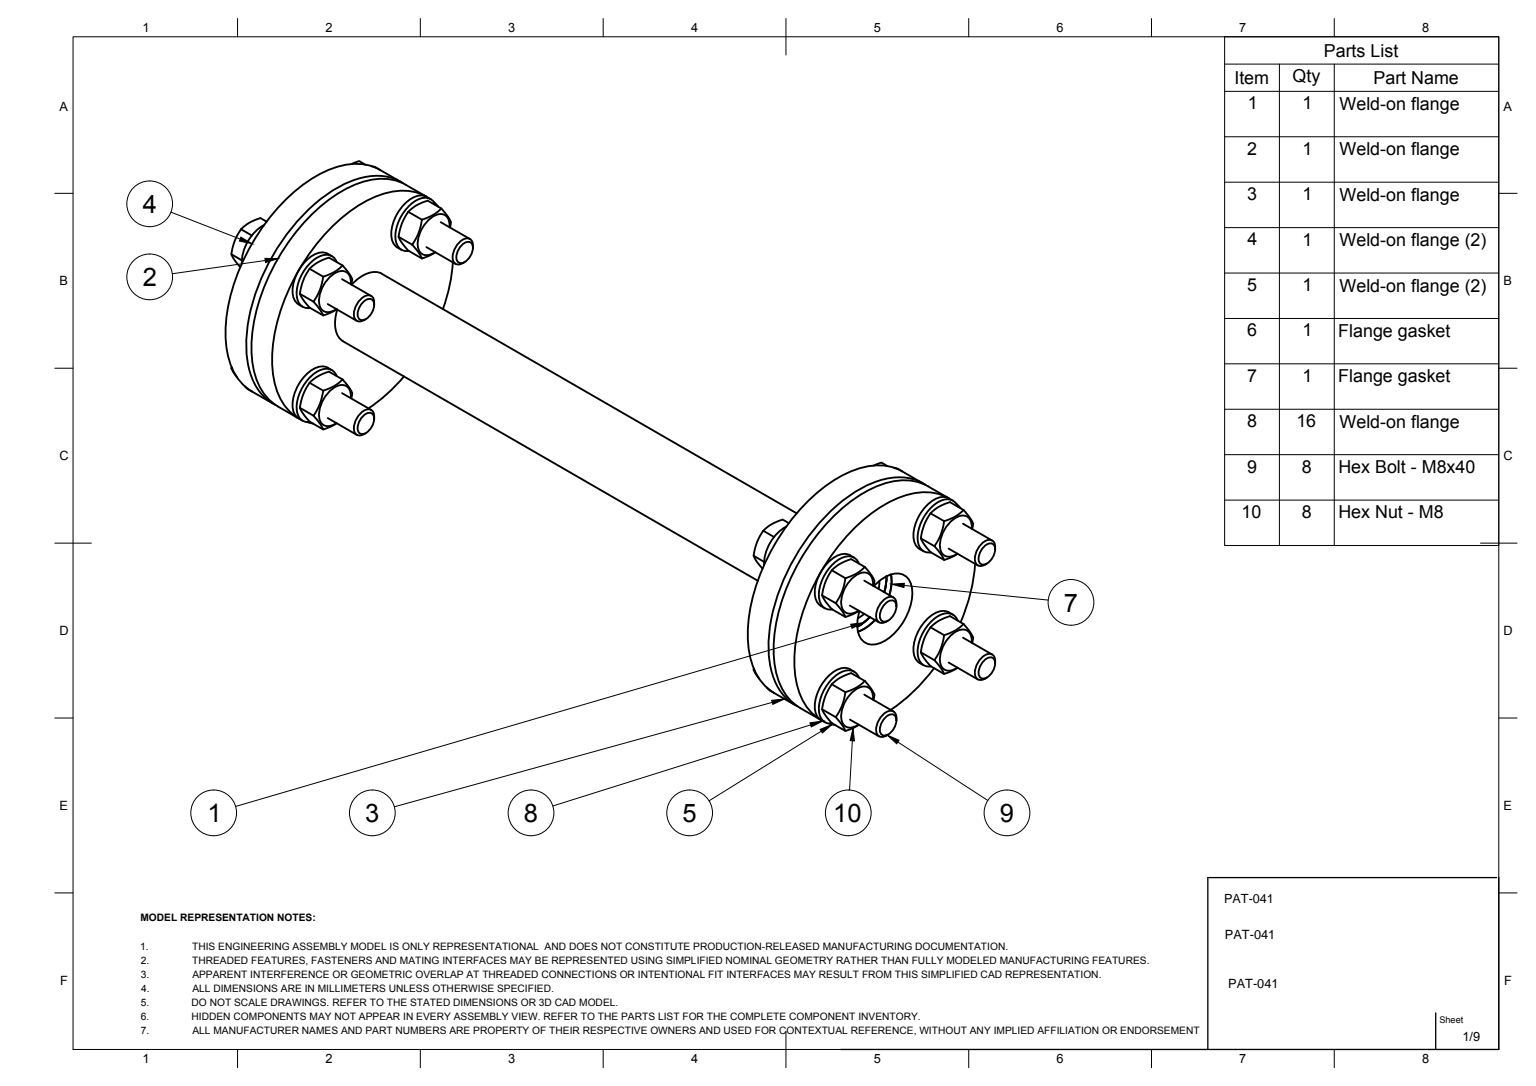
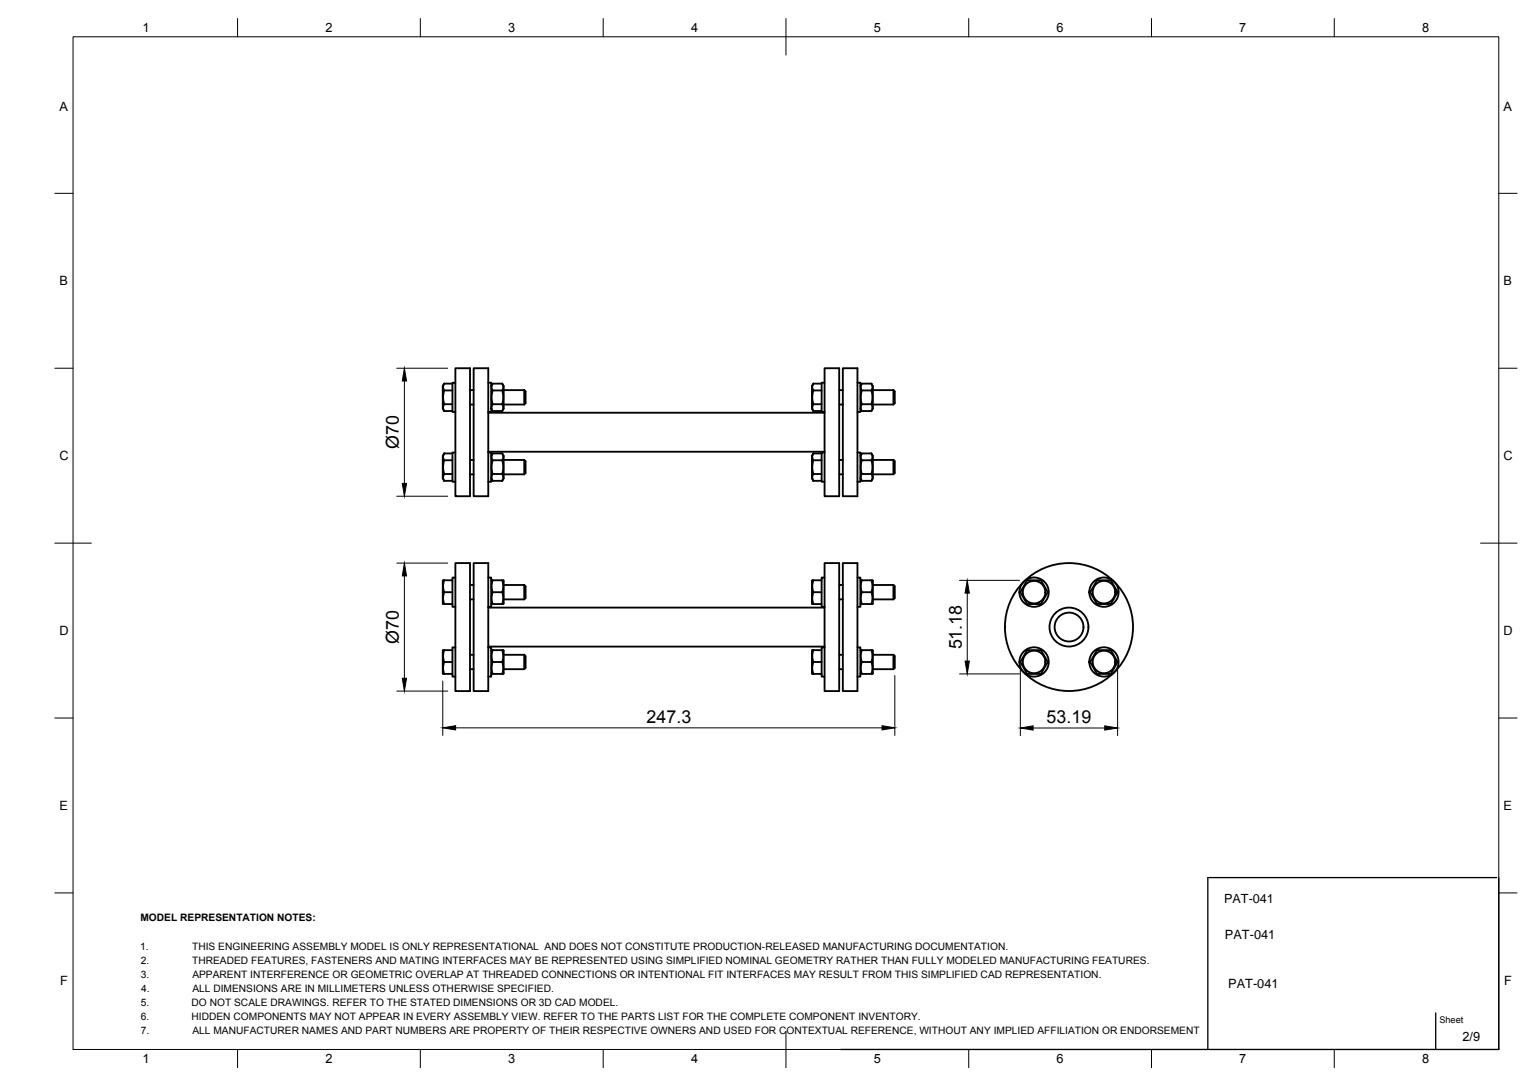
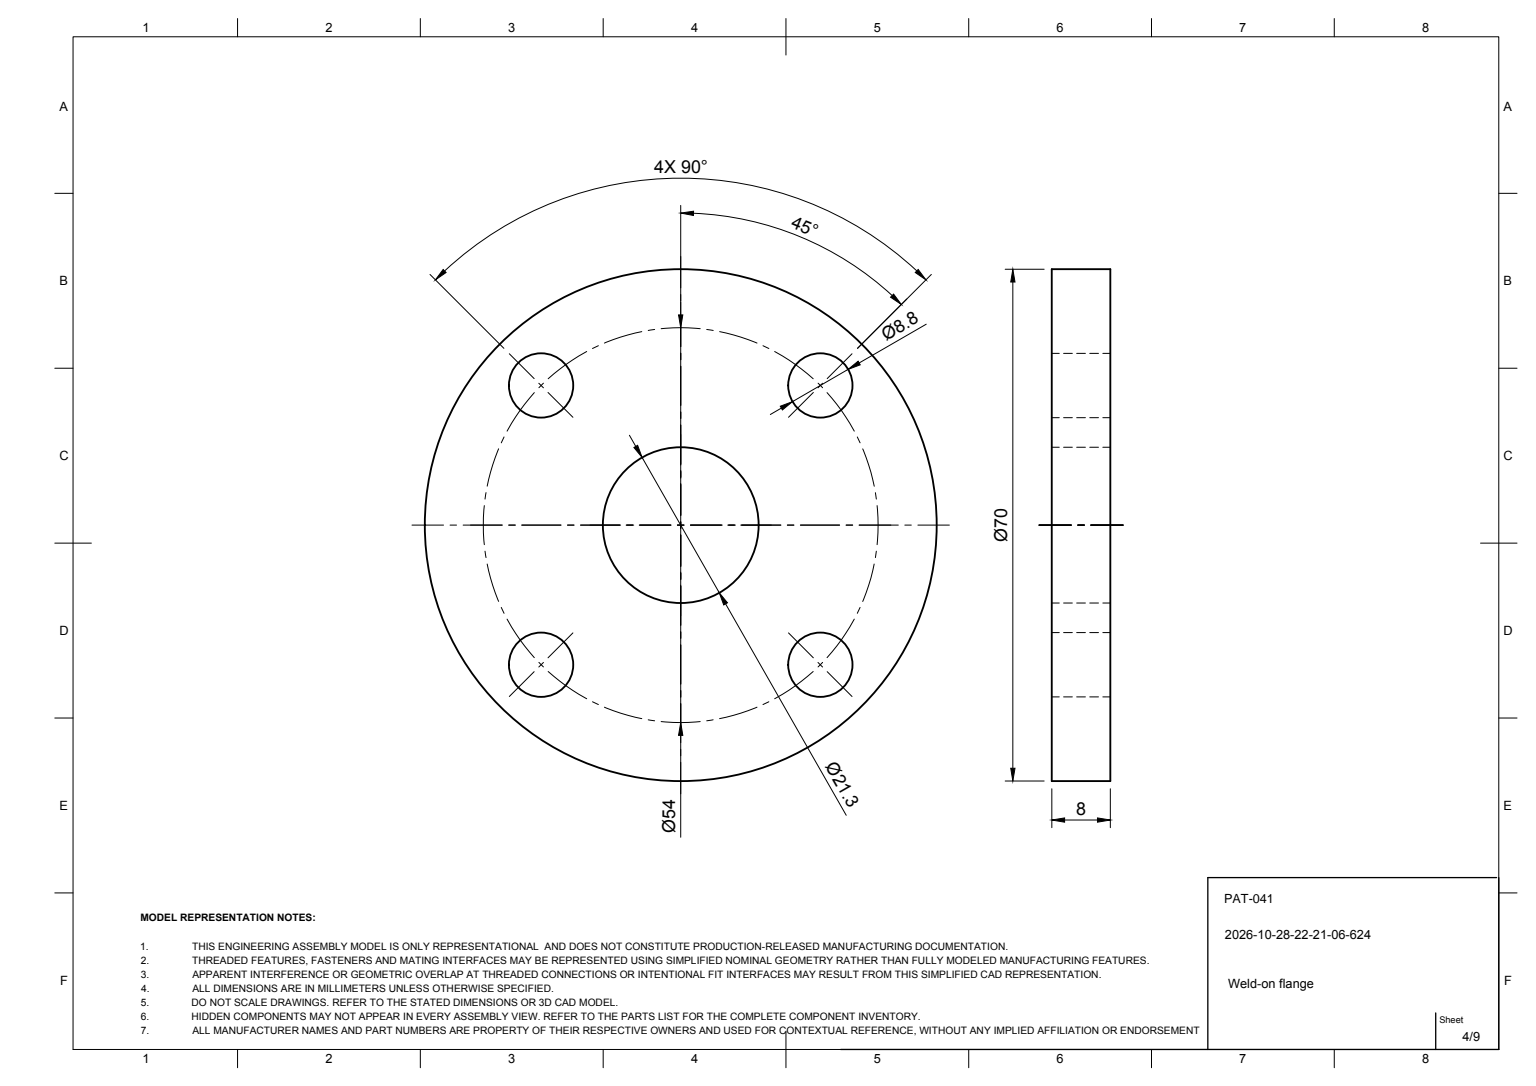
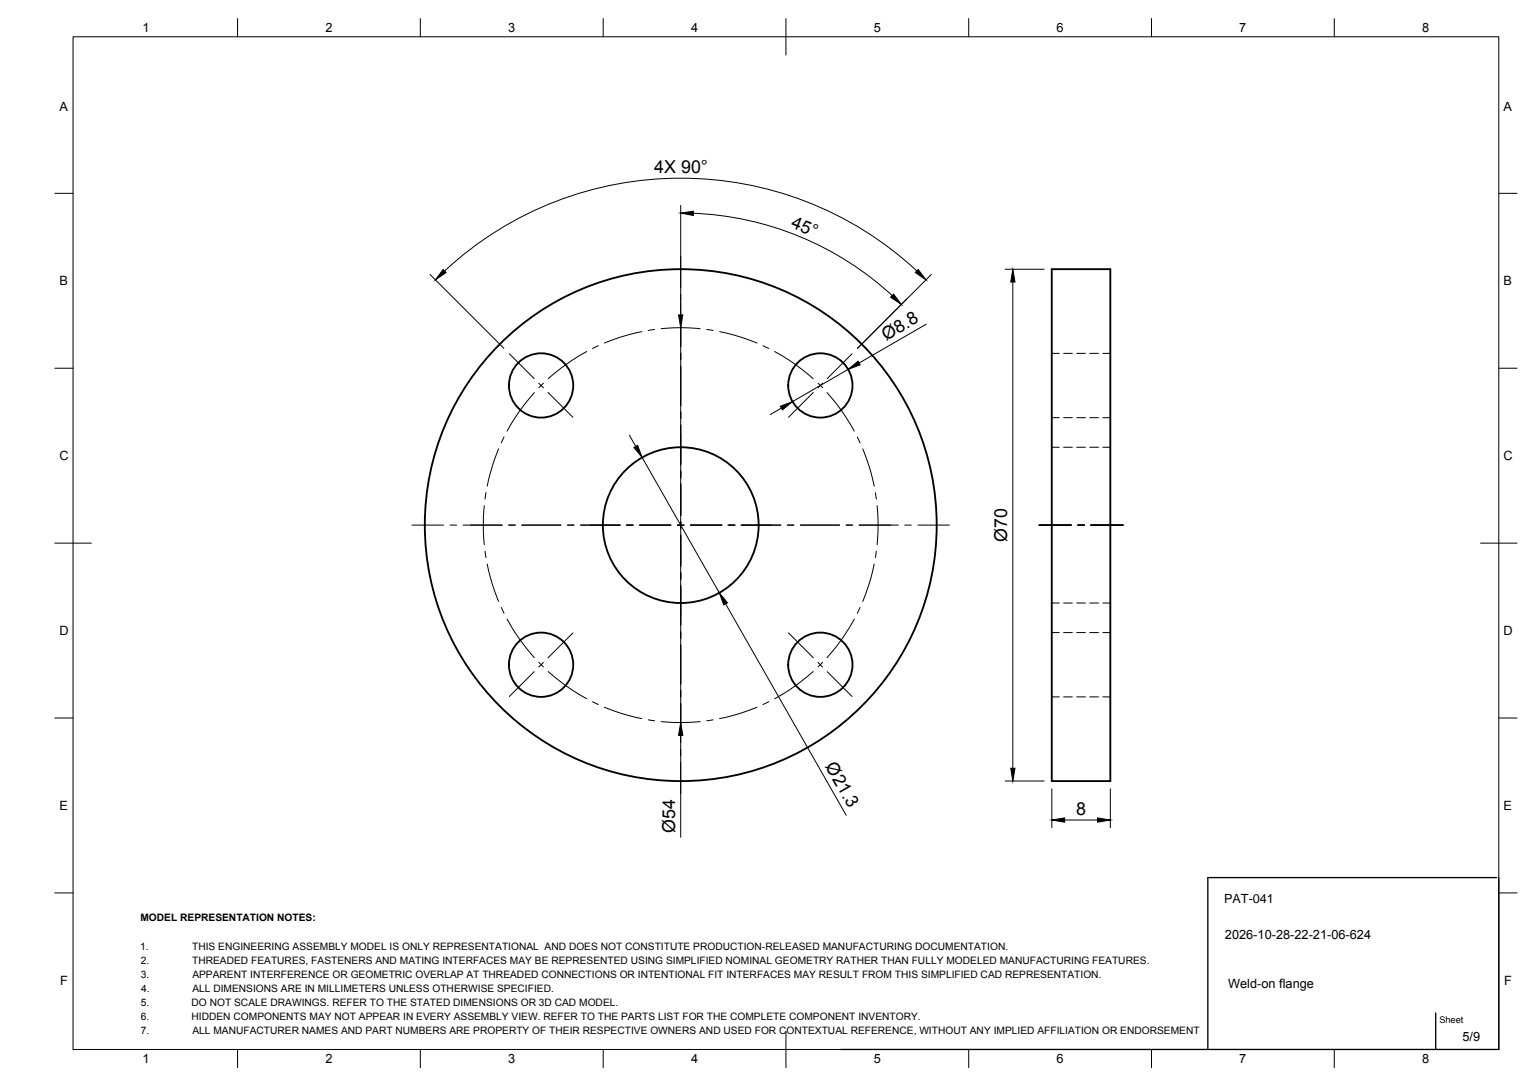
ISO-10303-21;
HEADER;
/* Generated by software containing ST-Developer
 * from STEP Tools, Inc. (www.steptools.com) 
 */

FILE_DESCRIPTION(
/* description */ ('PAT-041'),
/* implementation_level */ '2;1');

FILE_NAME(
/* name */ 'PAT-041',
/* time_stamp */ '2026-10-28T22:21:24-07:00',
/* author */ (''),
/* organization */ (''),
/* preprocessor_version */ 'ST-DEVELOPER v20.2',
/* originating_system */ 'Autodesk Translation Framework v15.17.0.0',
/* authorisation */ '');

FILE_SCHEMA (('AUTOMOTIVE_DESIGN { 1 0 10303 214 3 1 1 }'));
ENDSEC;

DATA;
#10=MECHANICAL_DESIGN_GEOMETRIC_PRESENTATION_REPRESENTATION('',(#209,#210,
#211,#212,#213,#214,#215,#216,#217,#218),#2507);
#11=ITEM_DEFINED_TRANSFORMATION($,$,#1451,#1604);
#12=ITEM_DEFINED_TRANSFORMATION($,$,#1460,#1605);
#13=ITEM_DEFINED_TRANSFORMATION($,$,#1481,#1606);
#14=ITEM_DEFINED_TRANSFORMATION($,$,#1502,#1607);
#15=ITEM_DEFINED_TRANSFORMATION($,$,#1523,#1608);
#16=ITEM_DEFINED_TRANSFORMATION($,$,#1544,#1609);
#17=ITEM_DEFINED_TRANSFORMATION($,$,#1553,#1610);
#18=ITEM_DEFINED_TRANSFORMATION($,$,#1579,#1611);
#19=ITEM_DEFINED_TRANSFORMATION($,$,#1562,#1612);
#20=ITEM_DEFINED_TRANSFORMATION($,$,#1579,#1613);
#21=ITEM_DEFINED_TRANSFORMATION($,$,#1588,#1614);
#22=ITEM_DEFINED_TRANSFORMATION($,$,#1579,#1615);
#23=ITEM_DEFINED_TRANSFORMATION($,$,#1562,#1616);
#24=ITEM_DEFINED_TRANSFORMATION($,$,#1579,#1617);
#25=ITEM_DEFINED_TRANSFORMATION($,$,#1588,#1618);
#26=ITEM_DEFINED_TRANSFORMATION($,$,#1579,#1619);
#27=ITEM_DEFINED_TRANSFORMATION($,$,#1562,#1620);
#28=ITEM_DEFINED_TRANSFORMATION($,$,#1579,#1621);
#29=ITEM_DEFINED_TRANSFORMATION($,$,#1588,#1622);
#30=ITEM_DEFINED_TRANSFORMATION($,$,#1579,#1623);
#31=ITEM_DEFINED_TRANSFORMATION($,$,#1562,#1624);
#32=ITEM_DEFINED_TRANSFORMATION($,$,#1579,#1625);
#33=ITEM_DEFINED_TRANSFORMATION($,$,#1588,#1626);
#34=ITEM_DEFINED_TRANSFORMATION($,$,#1579,#1627);
#35=ITEM_DEFINED_TRANSFORMATION($,$,#1562,#1628);
#36=ITEM_DEFINED_TRANSFORMATION($,$,#1579,#1629);
#37=ITEM_DEFINED_TRANSFORMATION($,$,#1588,#1630);
#38=ITEM_DEFINED_TRANSFORMATION($,$,#1579,#1631);
#39=ITEM_DEFINED_TRANSFORMATION($,$,#1562,#1632);
#40=ITEM_DEFINED_TRANSFORMATION($,$,#1579,#1633);
#41=ITEM_DEFINED_TRANSFORMATION($,$,#1588,#1634);
#42=ITEM_DEFINED_TRANSFORMATION($,$,#1579,#1635);
#43=ITEM_DEFINED_TRANSFORMATION($,$,#1562,#1636);
#44=ITEM_DEFINED_TRANSFORMATION($,$,#1579,#1637);
#45=ITEM_DEFINED_TRANSFORMATION($,$,#1588,#1638);
#46=ITEM_DEFINED_TRANSFORMATION($,$,#1579,#1639);
#47=ITEM_DEFINED_TRANSFORMATION($,$,#1562,#1640);
#48=ITEM_DEFINED_TRANSFORMATION($,$,#1579,#1641);
#49=ITEM_DEFINED_TRANSFORMATION($,$,#1588,#1642);
#50=(
REPRESENTATION_RELATIONSHIP($,$,#2574,#2573)
REPRESENTATION_RELATIONSHIP_WITH_TRANSFORMATION(#11)
SHAPE_REPRESENTATION_RELATIONSHIP()
);
#51=(
REPRESENTATION_RELATIONSHIP($,$,#2575,#2573)
REPRESENTATION_RELATIONSHIP_WITH_TRANSFORMATION(#12)
SHAPE_REPRESENTATION_RELATIONSHIP()
);
#52=(
REPRESENTATION_RELATIONSHIP($,$,#2576,#2573)
REPRESENTATION_RELATIONSHIP_WITH_TRANSFORMATION(#13)
SHAPE_REPRESENTATION_RELATIONSHIP()
);
#53=(
REPRESENTATION_RELATIONSHIP($,$,#2577,#2573)
REPRESENTATION_RELATIONSHIP_WITH_TRANSFORMATION(#14)
SHAPE_REPRESENTATION_RELATIONSHIP()
);
#54=(
REPRESENTATION_RELATIONSHIP($,$,#2578,#2573)
REPRESENTATION_RELATIONSHIP_WITH_TRANSFORMATION(#15)
SHAPE_REPRESENTATION_RELATIONSHIP()
);
#55=(
REPRESENTATION_RELATIONSHIP($,$,#2579,#2573)
REPRESENTATION_RELATIONSHIP_WITH_TRANSFORMATION(#16)
SHAPE_REPRESENTATION_RELATIONSHIP()
);
#56=(
REPRESENTATION_RELATIONSHIP($,$,#2580,#2573)
REPRESENTATION_RELATIONSHIP_WITH_TRANSFORMATION(#17)
SHAPE_REPRESENTATION_RELATIONSHIP()
);
#57=(
REPRESENTATION_RELATIONSHIP($,$,#2582,#2573)
REPRESENTATION_RELATIONSHIP_WITH_TRANSFORMATION(#18)
SHAPE_REPRESENTATION_RELATIONSHIP()
);
#58=(
REPRESENTATION_RELATIONSHIP($,$,#2581,#2573)
REPRESENTATION_RELATIONSHIP_WITH_TRANSFORMATION(#19)
SHAPE_REPRESENTATION_RELATIONSHIP()
);
#59=(
REPRESENTATION_RELATIONSHIP($,$,#2582,#2573)
REPRESENTATION_RELATIONSHIP_WITH_TRANSFORMATION(#20)
SHAPE_REPRESENTATION_RELATIONSHIP()
);
#60=(
REPRESENTATION_RELATIONSHIP($,$,#2583,#2573)
REPRESENTATION_RELATIONSHIP_WITH_TRANSFORMATION(#21)
SHAPE_REPRESENTATION_RELATIONSHIP()
);
#61=(
REPRESENTATION_RELATIONSHIP($,$,#2582,#2573)
REPRESENTATION_RELATIONSHIP_WITH_TRANSFORMATION(#22)
SHAPE_REPRESENTATION_RELATIONSHIP()
);
#62=(
REPRESENTATION_RELATIONSHIP($,$,#2581,#2573)
REPRESENTATION_RELATIONSHIP_WITH_TRANSFORMATION(#23)
SHAPE_REPRESENTATION_RELATIONSHIP()
);
#63=(
REPRESENTATION_RELATIONSHIP($,$,#2582,#2573)
REPRESENTATION_RELATIONSHIP_WITH_TRANSFORMATION(#24)
SHAPE_REPRESENTATION_RELATIONSHIP()
);
#64=(
REPRESENTATION_RELATIONSHIP($,$,#2583,#2573)
REPRESENTATION_RELATIONSHIP_WITH_TRANSFORMATION(#25)
SHAPE_REPRESENTATION_RELATIONSHIP()
);
#65=(
REPRESENTATION_RELATIONSHIP($,$,#2582,#2573)
REPRESENTATION_RELATIONSHIP_WITH_TRANSFORMATION(#26)
SHAPE_REPRESENTATION_RELATIONSHIP()
);
#66=(
REPRESENTATION_RELATIONSHIP($,$,#2581,#2573)
REPRESENTATION_RELATIONSHIP_WITH_TRANSFORMATION(#27)
SHAPE_REPRESENTATION_RELATIONSHIP()
);
#67=(
REPRESENTATION_RELATIONSHIP($,$,#2582,#2573)
REPRESENTATION_RELATIONSHIP_WITH_TRANSFORMATION(#28)
SHAPE_REPRESENTATION_RELATIONSHIP()
);
#68=(
REPRESENTATION_RELATIONSHIP($,$,#2583,#2573)
REPRESENTATION_RELATIONSHIP_WITH_TRANSFORMATION(#29)
SHAPE_REPRESENTATION_RELATIONSHIP()
);
#69=(
REPRESENTATION_RELATIONSHIP($,$,#2582,#2573)
REPRESENTATION_RELATIONSHIP_WITH_TRANSFORMATION(#30)
SHAPE_REPRESENTATION_RELATIONSHIP()
);
#70=(
REPRESENTATION_RELATIONSHIP($,$,#2581,#2573)
REPRESENTATION_RELATIONSHIP_WITH_TRANSFORMATION(#31)
SHAPE_REPRESENTATION_RELATIONSHIP()
);
#71=(
REPRESENTATION_RELATIONSHIP($,$,#2582,#2573)
REPRESENTATION_RELATIONSHIP_WITH_TRANSFORMATION(#32)
SHAPE_REPRESENTATION_RELATIONSHIP()
);
#72=(
REPRESENTATION_RELATIONSHIP($,$,#2583,#2573)
REPRESENTATION_RELATIONSHIP_WITH_TRANSFORMATION(#33)
SHAPE_REPRESENTATION_RELATIONSHIP()
);
#73=(
REPRESENTATION_RELATIONSHIP($,$,#2582,#2573)
REPRESENTATION_RELATIONSHIP_WITH_TRANSFORMATION(#34)
SHAPE_REPRESENTATION_RELATIONSHIP()
);
#74=(
REPRESENTATION_RELATIONSHIP($,$,#2581,#2573)
REPRESENTATION_RELATIONSHIP_WITH_TRANSFORMATION(#35)
SHAPE_REPRESENTATION_RELATIONSHIP()
);
#75=(
REPRESENTATION_RELATIONSHIP($,$,#2582,#2573)
REPRESENTATION_RELATIONSHIP_WITH_TRANSFORMATION(#36)
SHAPE_REPRESENTATION_RELATIONSHIP()
);
#76=(
REPRESENTATION_RELATIONSHIP($,$,#2583,#2573)
REPRESENTATION_RELATIONSHIP_WITH_TRANSFORMATION(#37)
SHAPE_REPRESENTATION_RELATIONSHIP()
);
#77=(
REPRESENTATION_RELATIONSHIP($,$,#2582,#2573)
REPRESENTATION_RELATIONSHIP_WITH_TRANSFORMATION(#38)
SHAPE_REPRESENTATION_RELATIONSHIP()
);
#78=(
REPRESENTATION_RELATIONSHIP($,$,#2581,#2573)
REPRESENTATION_RELATIONSHIP_WITH_TRANSFORMATION(#39)
SHAPE_REPRESENTATION_RELATIONSHIP()
);
#79=(
REPRESENTATION_RELATIONSHIP($,$,#2582,#2573)
REPRESENTATION_RELATIONSHIP_WITH_TRANSFORMATION(#40)
SHAPE_REPRESENTATION_RELATIONSHIP()
);
#80=(
REPRESENTATION_RELATIONSHIP($,$,#2583,#2573)
REPRESENTATION_RELATIONSHIP_WITH_TRANSFORMATION(#41)
SHAPE_REPRESENTATION_RELATIONSHIP()
);
#81=(
REPRESENTATION_RELATIONSHIP($,$,#2582,#2573)
REPRESENTATION_RELATIONSHIP_WITH_TRANSFORMATION(#42)
SHAPE_REPRESENTATION_RELATIONSHIP()
);
#82=(
REPRESENTATION_RELATIONSHIP($,$,#2581,#2573)
REPRESENTATION_RELATIONSHIP_WITH_TRANSFORMATION(#43)
SHAPE_REPRESENTATION_RELATIONSHIP()
);
#83=(
REPRESENTATION_RELATIONSHIP($,$,#2582,#2573)
REPRESENTATION_RELATIONSHIP_WITH_TRANSFORMATION(#44)
SHAPE_REPRESENTATION_RELATIONSHIP()
);
#84=(
REPRESENTATION_RELATIONSHIP($,$,#2583,#2573)
REPRESENTATION_RELATIONSHIP_WITH_TRANSFORMATION(#45)
SHAPE_REPRESENTATION_RELATIONSHIP()
);
#85=(
REPRESENTATION_RELATIONSHIP($,$,#2582,#2573)
REPRESENTATION_RELATIONSHIP_WITH_TRANSFORMATION(#46)
SHAPE_REPRESENTATION_RELATIONSHIP()
);
#86=(
REPRESENTATION_RELATIONSHIP($,$,#2581,#2573)
REPRESENTATION_RELATIONSHIP_WITH_TRANSFORMATION(#47)
SHAPE_REPRESENTATION_RELATIONSHIP()
);
#87=(
REPRESENTATION_RELATIONSHIP($,$,#2582,#2573)
REPRESENTATION_RELATIONSHIP_WITH_TRANSFORMATION(#48)
SHAPE_REPRESENTATION_RELATIONSHIP()
);
#88=(
REPRESENTATION_RELATIONSHIP($,$,#2583,#2573)
REPRESENTATION_RELATIONSHIP_WITH_TRANSFORMATION(#49)
SHAPE_REPRESENTATION_RELATIONSHIP()
);
#89=CONTEXT_DEPENDENT_SHAPE_REPRESENTATION(#50,#2534);
#90=CONTEXT_DEPENDENT_SHAPE_REPRESENTATION(#51,#2535);
#91=CONTEXT_DEPENDENT_SHAPE_REPRESENTATION(#52,#2536);
#92=CONTEXT_DEPENDENT_SHAPE_REPRESENTATION(#53,#2537);
#93=CONTEXT_DEPENDENT_SHAPE_REPRESENTATION(#54,#2538);
#94=CONTEXT_DEPENDENT_SHAPE_REPRESENTATION(#55,#2539);
#95=CONTEXT_DEPENDENT_SHAPE_REPRESENTATION(#56,#2540);
#96=CONTEXT_DEPENDENT_SHAPE_REPRESENTATION(#57,#2541);
#97=CONTEXT_DEPENDENT_SHAPE_REPRESENTATION(#58,#2542);
#98=CONTEXT_DEPENDENT_SHAPE_REPRESENTATION(#59,#2543);
#99=CONTEXT_DEPENDENT_SHAPE_REPRESENTATION(#60,#2544);
#100=CONTEXT_DEPENDENT_SHAPE_REPRESENTATION(#61,#2545);
#101=CONTEXT_DEPENDENT_SHAPE_REPRESENTATION(#62,#2546);
#102=CONTEXT_DEPENDENT_SHAPE_REPRESENTATION(#63,#2547);
#103=CONTEXT_DEPENDENT_SHAPE_REPRESENTATION(#64,#2548);
#104=CONTEXT_DEPENDENT_SHAPE_REPRESENTATION(#65,#2549);
#105=CONTEXT_DEPENDENT_SHAPE_REPRESENTATION(#66,#2550);
#106=CONTEXT_DEPENDENT_SHAPE_REPRESENTATION(#67,#2551);
#107=CONTEXT_DEPENDENT_SHAPE_REPRESENTATION(#68,#2552);
#108=CONTEXT_DEPENDENT_SHAPE_REPRESENTATION(#69,#2553);
#109=CONTEXT_DEPENDENT_SHAPE_REPRESENTATION(#70,#2554);
#110=CONTEXT_DEPENDENT_SHAPE_REPRESENTATION(#71,#2555);
#111=CONTEXT_DEPENDENT_SHAPE_REPRESENTATION(#72,#2556);
#112=CONTEXT_DEPENDENT_SHAPE_REPRESENTATION(#73,#2557);
#113=CONTEXT_DEPENDENT_SHAPE_REPRESENTATION(#74,#2558);
#114=CONTEXT_DEPENDENT_SHAPE_REPRESENTATION(#75,#2559);
#115=CONTEXT_DEPENDENT_SHAPE_REPRESENTATION(#76,#2560);
#116=CONTEXT_DEPENDENT_SHAPE_REPRESENTATION(#77,#2561);
#117=CONTEXT_DEPENDENT_SHAPE_REPRESENTATION(#78,#2562);
#118=CONTEXT_DEPENDENT_SHAPE_REPRESENTATION(#79,#2563);
#119=CONTEXT_DEPENDENT_SHAPE_REPRESENTATION(#80,#2564);
#120=CONTEXT_DEPENDENT_SHAPE_REPRESENTATION(#81,#2565);
#121=CONTEXT_DEPENDENT_SHAPE_REPRESENTATION(#82,#2566);
#122=CONTEXT_DEPENDENT_SHAPE_REPRESENTATION(#83,#2567);
#123=CONTEXT_DEPENDENT_SHAPE_REPRESENTATION(#84,#2568);
#124=CONTEXT_DEPENDENT_SHAPE_REPRESENTATION(#85,#2569);
#125=CONTEXT_DEPENDENT_SHAPE_REPRESENTATION(#86,#2570);
#126=CONTEXT_DEPENDENT_SHAPE_REPRESENTATION(#87,#2571);
#127=CONTEXT_DEPENDENT_SHAPE_REPRESENTATION(#88,#2572);
#128=NEXT_ASSEMBLY_USAGE_OCCURRENCE('Pipe spool:1','Pipe spool:1',
'Pipe spool:1',#2585,#2586,'Pipe spool:1');
#129=NEXT_ASSEMBLY_USAGE_OCCURRENCE('Weld-on flange:1',
'Weld-on flange:1','Weld-on flange:1',#2585,#2587,'Weld-on flange:1');
#130=NEXT_ASSEMBLY_USAGE_OCCURRENCE('Weld-on flange (1):1',
'Weld-on flange (1):1','Weld-on flange (1):1',#2585,#2588,
'Weld-on flange (1):1');
#131=NEXT_ASSEMBLY_USAGE_OCCURRENCE('Weld-on flange (2):1',
'Weld-on flange (2):1','Weld-on flange (2):1',#2585,#2589,
'Weld-on flange (2):1');
#132=NEXT_ASSEMBLY_USAGE_OCCURRENCE('Weld-on flange (3):1',
'Weld-on flange (3):1','Weld-on flange (3):1',#2585,#2590,
'Weld-on flange (3):1');
#133=NEXT_ASSEMBLY_USAGE_OCCURRENCE('Flange gasket:1','Flange gasket:1',
'Flange gasket:1',#2585,#2591,'Flange gasket:1');
#134=NEXT_ASSEMBLY_USAGE_OCCURRENCE('Flange gasket (1):1',
'Flange gasket (1):1','Flange gasket (1):1',#2585,#2592,
'Flange gasket (1):1');
#135=NEXT_ASSEMBLY_USAGE_OCCURRENCE('Flat Washer - M8:1',
'Flat Washer - M8:1','Flat Washer - M8:1',#2585,#2594,
'Flat Washer - M8:1');
#136=NEXT_ASSEMBLY_USAGE_OCCURRENCE('Hex Bolt - M8x40:1',
'Hex Bolt - M8x40:1','Hex Bolt - M8x40:1',#2585,#2593,
'Hex Bolt - M8x40:1');
#137=NEXT_ASSEMBLY_USAGE_OCCURRENCE('Flat Washer - M8:2',
'Flat Washer - M8:2','Flat Washer - M8:2',#2585,#2594,
'Flat Washer - M8:2');
#138=NEXT_ASSEMBLY_USAGE_OCCURRENCE('Hex Nut - M8:1','Hex Nut - M8:1',
'Hex Nut - M8:1',#2585,#2595,'Hex Nut - M8:1');
#139=NEXT_ASSEMBLY_USAGE_OCCURRENCE('Flat Washer - M8:3',
'Flat Washer - M8:3','Flat Washer - M8:3',#2585,#2594,
'Flat Washer - M8:3');
#140=NEXT_ASSEMBLY_USAGE_OCCURRENCE('Hex Bolt - M8x40:2',
'Hex Bolt - M8x40:2','Hex Bolt - M8x40:2',#2585,#2593,
'Hex Bolt - M8x40:2');
#141=NEXT_ASSEMBLY_USAGE_OCCURRENCE('Flat Washer - M8:4',
'Flat Washer - M8:4','Flat Washer - M8:4',#2585,#2594,
'Flat Washer - M8:4');
#142=NEXT_ASSEMBLY_USAGE_OCCURRENCE('Hex Nut - M8:2','Hex Nut - M8:2',
'Hex Nut - M8:2',#2585,#2595,'Hex Nut - M8:2');
#143=NEXT_ASSEMBLY_USAGE_OCCURRENCE('Flat Washer - M8:5',
'Flat Washer - M8:5','Flat Washer - M8:5',#2585,#2594,
'Flat Washer - M8:5');
#144=NEXT_ASSEMBLY_USAGE_OCCURRENCE('Hex Bolt - M8x40:3',
'Hex Bolt - M8x40:3','Hex Bolt - M8x40:3',#2585,#2593,
'Hex Bolt - M8x40:3');
#145=NEXT_ASSEMBLY_USAGE_OCCURRENCE('Flat Washer - M8:6',
'Flat Washer - M8:6','Flat Washer - M8:6',#2585,#2594,
'Flat Washer - M8:6');
#146=NEXT_ASSEMBLY_USAGE_OCCURRENCE('Hex Nut - M8:3','Hex Nut - M8:3',
'Hex Nut - M8:3',#2585,#2595,'Hex Nut - M8:3');
#147=NEXT_ASSEMBLY_USAGE_OCCURRENCE('Flat Washer - M8:7',
'Flat Washer - M8:7','Flat Washer - M8:7',#2585,#2594,
'Flat Washer - M8:7');
#148=NEXT_ASSEMBLY_USAGE_OCCURRENCE('Hex Bolt - M8x40:4',
'Hex Bolt - M8x40:4','Hex Bolt - M8x40:4',#2585,#2593,
'Hex Bolt - M8x40:4');
#149=NEXT_ASSEMBLY_USAGE_OCCURRENCE('Flat Washer - M8:8',
'Flat Washer - M8:8','Flat Washer - M8:8',#2585,#2594,
'Flat Washer - M8:8');
#150=NEXT_ASSEMBLY_USAGE_OCCURRENCE('Hex Nut - M8:4','Hex Nut - M8:4',
'Hex Nut - M8:4',#2585,#2595,'Hex Nut - M8:4');
#151=NEXT_ASSEMBLY_USAGE_OCCURRENCE('Flat Washer - M8:9',
'Flat Washer - M8:9','Flat Washer - M8:9',#2585,#2594,
'Flat Washer - M8:9');
#152=NEXT_ASSEMBLY_USAGE_OCCURRENCE('Hex Bolt - M8x40:5',
'Hex Bolt - M8x40:5','Hex Bolt - M8x40:5',#2585,#2593,
'Hex Bolt - M8x40:5');
#153=NEXT_ASSEMBLY_USAGE_OCCURRENCE('Flat Washer - M8:10',
'Flat Washer - M8:10','Flat Washer - M8:10',#2585,#2594,
'Flat Washer - M8:10');
#154=NEXT_ASSEMBLY_USAGE_OCCURRENCE('Hex Nut - M8:5','Hex Nut - M8:5',
'Hex Nut - M8:5',#2585,#2595,'Hex Nut - M8:5');
#155=NEXT_ASSEMBLY_USAGE_OCCURRENCE('Flat Washer - M8:11',
'Flat Washer - M8:11','Flat Washer - M8:11',#2585,#2594,
'Flat Washer - M8:11');
#156=NEXT_ASSEMBLY_USAGE_OCCURRENCE('Hex Bolt - M8x40:6',
'Hex Bolt - M8x40:6','Hex Bolt - M8x40:6',#2585,#2593,
'Hex Bolt - M8x40:6');
#157=NEXT_ASSEMBLY_USAGE_OCCURRENCE('Flat Washer - M8:12',
'Flat Washer - M8:12','Flat Washer - M8:12',#2585,#2594,
'Flat Washer - M8:12');
#158=NEXT_ASSEMBLY_USAGE_OCCURRENCE('Hex Nut - M8:6','Hex Nut - M8:6',
'Hex Nut - M8:6',#2585,#2595,'Hex Nut - M8:6');
#159=NEXT_ASSEMBLY_USAGE_OCCURRENCE('Flat Washer - M8:13',
'Flat Washer - M8:13','Flat Washer - M8:13',#2585,#2594,
'Flat Washer - M8:13');
#160=NEXT_ASSEMBLY_USAGE_OCCURRENCE('Hex Bolt - M8x40:7',
'Hex Bolt - M8x40:7','Hex Bolt - M8x40:7',#2585,#2593,
'Hex Bolt - M8x40:7');
#161=NEXT_ASSEMBLY_USAGE_OCCURRENCE('Flat Washer - M8:14',
'Flat Washer - M8:14','Flat Washer - M8:14',#2585,#2594,
'Flat Washer - M8:14');
#162=NEXT_ASSEMBLY_USAGE_OCCURRENCE('Hex Nut - M8:7','Hex Nut - M8:7',
'Hex Nut - M8:7',#2585,#2595,'Hex Nut - M8:7');
#163=NEXT_ASSEMBLY_USAGE_OCCURRENCE('Flat Washer - M8:15',
'Flat Washer - M8:15','Flat Washer - M8:15',#2585,#2594,
'Flat Washer - M8:15');
#164=NEXT_ASSEMBLY_USAGE_OCCURRENCE('Hex Bolt - M8x40:8',
'Hex Bolt - M8x40:8','Hex Bolt - M8x40:8',#2585,#2593,
'Hex Bolt - M8x40:8');
#165=NEXT_ASSEMBLY_USAGE_OCCURRENCE('Flat Washer - M8:16',
'Flat Washer - M8:16','Flat Washer - M8:16',#2585,#2594,
'Flat Washer - M8:16');
#166=NEXT_ASSEMBLY_USAGE_OCCURRENCE('Hex Nut - M8:8','Hex Nut - M8:8',
'Hex Nut - M8:8',#2585,#2595,'Hex Nut - M8:8');
#167=(
BOUNDED_CURVE()
B_SPLINE_CURVE(2,(#2305,#2306,#2307),.UNSPECIFIED.,.F.,.F.)
B_SPLINE_CURVE_WITH_KNOTS((3,3),(0.14973948338295,0.97160236658079),
 .UNSPECIFIED.)
CURVE()
GEOMETRIC_REPRESENTATION_ITEM()
RATIONAL_B_SPLINE_CURVE((1.07140024848292,1.23714644374248,1.07140024848292))
REPRESENTATION_ITEM('')
);
#168=(
BOUNDED_CURVE()
B_SPLINE_CURVE(2,(#2309,#2310,#2311),.UNSPECIFIED.,.F.,.F.)
B_SPLINE_CURVE_WITH_KNOTS((3,3),(0.14973948338295,0.97160236658079),
 .UNSPECIFIED.)
CURVE()
GEOMETRIC_REPRESENTATION_ITEM()
RATIONAL_B_SPLINE_CURVE((1.07140024848292,1.23714644374248,1.07140024848292))
REPRESENTATION_ITEM('')
);
#169=(
BOUNDED_CURVE()
B_SPLINE_CURVE(2,(#2313,#2314,#2315),.UNSPECIFIED.,.F.,.F.)
B_SPLINE_CURVE_WITH_KNOTS((3,3),(0.14973948338295,0.97160236658079),
 .UNSPECIFIED.)
CURVE()
GEOMETRIC_REPRESENTATION_ITEM()
RATIONAL_B_SPLINE_CURVE((1.07140024848292,1.23714644374248,1.07140024848292))
REPRESENTATION_ITEM('')
);
#170=(
BOUNDED_CURVE()
B_SPLINE_CURVE(2,(#2317,#2318,#2319),.UNSPECIFIED.,.F.,.F.)
B_SPLINE_CURVE_WITH_KNOTS((3,3),(0.149739483382949,0.971602366580789),
 .UNSPECIFIED.)
CURVE()
GEOMETRIC_REPRESENTATION_ITEM()
RATIONAL_B_SPLINE_CURVE((1.07140024848292,1.23714644374248,1.07140024848292))
REPRESENTATION_ITEM('')
);
#171=(
BOUNDED_CURVE()
B_SPLINE_CURVE(2,(#2321,#2322,#2323),.UNSPECIFIED.,.F.,.F.)
B_SPLINE_CURVE_WITH_KNOTS((3,3),(0.14973948338295,0.971602366580789),
 .UNSPECIFIED.)
CURVE()
GEOMETRIC_REPRESENTATION_ITEM()
RATIONAL_B_SPLINE_CURVE((1.07140024848292,1.23714644374248,1.07140024848292))
REPRESENTATION_ITEM('')
);
#172=(
BOUNDED_CURVE()
B_SPLINE_CURVE(2,(#2324,#2325,#2326),.UNSPECIFIED.,.F.,.F.)
B_SPLINE_CURVE_WITH_KNOTS((3,3),(0.14973948338295,0.97160236658079),
 .UNSPECIFIED.)
CURVE()
GEOMETRIC_REPRESENTATION_ITEM()
RATIONAL_B_SPLINE_CURVE((1.07140024848292,1.23714644374248,1.07140024848292))
REPRESENTATION_ITEM('')
);
#173=(
BOUNDED_CURVE()
B_SPLINE_CURVE(2,(#2372,#2373,#2374),.UNSPECIFIED.,.F.,.F.)
B_SPLINE_CURVE_WITH_KNOTS((3,3),(0.14973948338295,0.97160236658079),
 .UNSPECIFIED.)
CURVE()
GEOMETRIC_REPRESENTATION_ITEM()
RATIONAL_B_SPLINE_CURVE((1.07140024848292,1.23714644374248,1.07140024848292))
REPRESENTATION_ITEM('')
);
#174=(
BOUNDED_CURVE()
B_SPLINE_CURVE(2,(#2376,#2377,#2378),.UNSPECIFIED.,.F.,.F.)
B_SPLINE_CURVE_WITH_KNOTS((3,3),(0.14973948338295,0.971602366580789),
 .UNSPECIFIED.)
CURVE()
GEOMETRIC_REPRESENTATION_ITEM()
RATIONAL_B_SPLINE_CURVE((1.07140024848292,1.23714644374248,1.07140024848292))
REPRESENTATION_ITEM('')
);
#175=(
BOUNDED_CURVE()
B_SPLINE_CURVE(2,(#2383,#2384,#2385),.UNSPECIFIED.,.F.,.F.)
B_SPLINE_CURVE_WITH_KNOTS((3,3),(0.14973948338295,0.97160236658079),
 .UNSPECIFIED.)
CURVE()
GEOMETRIC_REPRESENTATION_ITEM()
RATIONAL_B_SPLINE_CURVE((1.07140024848292,1.23714644374248,1.07140024848292))
REPRESENTATION_ITEM('')
);
#176=(
BOUNDED_CURVE()
B_SPLINE_CURVE(2,(#2387,#2388,#2389),.UNSPECIFIED.,.F.,.F.)
B_SPLINE_CURVE_WITH_KNOTS((3,3),(0.14973948338295,0.97160236658079),
 .UNSPECIFIED.)
CURVE()
GEOMETRIC_REPRESENTATION_ITEM()
RATIONAL_B_SPLINE_CURVE((1.07140024848292,1.23714644374248,1.07140024848292))
REPRESENTATION_ITEM('')
);
#177=(
BOUNDED_CURVE()
B_SPLINE_CURVE(2,(#2391,#2392,#2393),.UNSPECIFIED.,.F.,.F.)
B_SPLINE_CURVE_WITH_KNOTS((3,3),(0.14973948338295,0.971602366580789),
 .UNSPECIFIED.)
CURVE()
GEOMETRIC_REPRESENTATION_ITEM()
RATIONAL_B_SPLINE_CURVE((1.07140024848292,1.23714644374248,1.07140024848292))
REPRESENTATION_ITEM('')
);
#178=(
BOUNDED_CURVE()
B_SPLINE_CURVE(2,(#2394,#2395,#2396),.UNSPECIFIED.,.F.,.F.)
B_SPLINE_CURVE_WITH_KNOTS((3,3),(0.14973948338295,0.97160236658079),
 .UNSPECIFIED.)
CURVE()
GEOMETRIC_REPRESENTATION_ITEM()
RATIONAL_B_SPLINE_CURVE((1.07140024848292,1.23714644374248,1.07140024848292))
REPRESENTATION_ITEM('')
);
#179=(
BOUNDED_CURVE()
B_SPLINE_CURVE(2,(#2403,#2404,#2405),.UNSPECIFIED.,.F.,.F.)
B_SPLINE_CURVE_WITH_KNOTS((3,3),(0.14973948338295,0.97160236658079),
 .UNSPECIFIED.)
CURVE()
GEOMETRIC_REPRESENTATION_ITEM()
RATIONAL_B_SPLINE_CURVE((1.07140024848292,1.23714644374248,1.07140024848292))
REPRESENTATION_ITEM('')
);
#180=(
BOUNDED_CURVE()
B_SPLINE_CURVE(2,(#2407,#2408,#2409),.UNSPECIFIED.,.F.,.F.)
B_SPLINE_CURVE_WITH_KNOTS((3,3),(0.14973948338295,0.97160236658079),
 .UNSPECIFIED.)
CURVE()
GEOMETRIC_REPRESENTATION_ITEM()
RATIONAL_B_SPLINE_CURVE((1.07140024848292,1.23714644374248,1.07140024848292))
REPRESENTATION_ITEM('')
);
#181=(
BOUNDED_CURVE()
B_SPLINE_CURVE(2,(#2411,#2412,#2413),.UNSPECIFIED.,.F.,.F.)
B_SPLINE_CURVE_WITH_KNOTS((3,3),(0.14973948338295,0.971602366580789),
 .UNSPECIFIED.)
CURVE()
GEOMETRIC_REPRESENTATION_ITEM()
RATIONAL_B_SPLINE_CURVE((1.07140024848292,1.23714644374248,1.07140024848292))
REPRESENTATION_ITEM('')
);
#182=(
BOUNDED_CURVE()
B_SPLINE_CURVE(2,(#2415,#2416,#2417),.UNSPECIFIED.,.F.,.F.)
B_SPLINE_CURVE_WITH_KNOTS((3,3),(0.14973948338295,0.97160236658079),
 .UNSPECIFIED.)
CURVE()
GEOMETRIC_REPRESENTATION_ITEM()
RATIONAL_B_SPLINE_CURVE((1.07140024848292,1.23714644374248,1.07140024848292))
REPRESENTATION_ITEM('')
);
#183=(
BOUNDED_CURVE()
B_SPLINE_CURVE(2,(#2419,#2420,#2421),.UNSPECIFIED.,.F.,.F.)
B_SPLINE_CURVE_WITH_KNOTS((3,3),(0.14973948338295,0.97160236658079),
 .UNSPECIFIED.)
CURVE()
GEOMETRIC_REPRESENTATION_ITEM()
RATIONAL_B_SPLINE_CURVE((1.07140024848292,1.23714644374248,1.07140024848292))
REPRESENTATION_ITEM('')
);
#184=(
BOUNDED_CURVE()
B_SPLINE_CURVE(2,(#2422,#2423,#2424),.UNSPECIFIED.,.F.,.F.)
B_SPLINE_CURVE_WITH_KNOTS((3,3),(0.14973948338295,0.971602366580789),
 .UNSPECIFIED.)
CURVE()
GEOMETRIC_REPRESENTATION_ITEM()
RATIONAL_B_SPLINE_CURVE((1.07140024848292,1.23714644374248,1.07140024848292))
REPRESENTATION_ITEM('')
);
#185=CONICAL_SURFACE('',#1566,0.36,0.785398163397451);
#186=CONICAL_SURFACE('',#1569,0.734027674973257,1.0471975511966);
#187=CONICAL_SURFACE('',#1589,0.734027674973257,1.0471975511966);
#188=CONICAL_SURFACE('',#1591,0.734027674973257,1.0471975511966);
#189=SHAPE_REPRESENTATION_RELATIONSHIP('SRR','None',#2574,#199);
#190=SHAPE_REPRESENTATION_RELATIONSHIP('SRR','None',#2575,#200);
#191=SHAPE_REPRESENTATION_RELATIONSHIP('SRR','None',#2576,#201);
#192=SHAPE_REPRESENTATION_RELATIONSHIP('SRR','None',#2577,#202);
#193=SHAPE_REPRESENTATION_RELATIONSHIP('SRR','None',#2578,#203);
#194=SHAPE_REPRESENTATION_RELATIONSHIP('SRR','None',#2579,#204);
#195=SHAPE_REPRESENTATION_RELATIONSHIP('SRR','None',#2580,#205);
#196=SHAPE_REPRESENTATION_RELATIONSHIP('SRR','None',#2581,#206);
#197=SHAPE_REPRESENTATION_RELATIONSHIP('SRR','None',#2582,#207);
#198=SHAPE_REPRESENTATION_RELATIONSHIP('SRR','None',#2583,#208);
#199=ADVANCED_BREP_SHAPE_REPRESENTATION('',(#219),#2497);
#200=ADVANCED_BREP_SHAPE_REPRESENTATION('',(#220),#2498);
#201=ADVANCED_BREP_SHAPE_REPRESENTATION('',(#221),#2499);
#202=ADVANCED_BREP_SHAPE_REPRESENTATION('',(#222),#2500);
#203=ADVANCED_BREP_SHAPE_REPRESENTATION('',(#223),#2501);
#204=ADVANCED_BREP_SHAPE_REPRESENTATION('',(#224),#2502);
#205=ADVANCED_BREP_SHAPE_REPRESENTATION('',(#225),#2503);
#206=ADVANCED_BREP_SHAPE_REPRESENTATION('',(#226),#2504);
#207=ADVANCED_BREP_SHAPE_REPRESENTATION('',(#227),#2505);
#208=ADVANCED_BREP_SHAPE_REPRESENTATION('',(#228),#2506);
#209=STYLED_ITEM('',(#2708),#219);
#210=STYLED_ITEM('',(#2687),#220);
#211=STYLED_ITEM('',(#2687),#221);
#212=STYLED_ITEM('',(#2687),#222);
#213=STYLED_ITEM('',(#2687),#223);
#214=STYLED_ITEM('',(#2708),#224);
#215=STYLED_ITEM('',(#2708),#225);
#216=STYLED_ITEM('',(#2701),#226);
#217=STYLED_ITEM('',(#2701),#227);
#218=STYLED_ITEM('',(#2701),#228);
#219=MANIFOLD_SOLID_BREP('Body1',#1329);
#220=MANIFOLD_SOLID_BREP('Body1',#1330);
#221=MANIFOLD_SOLID_BREP('Body1',#1331);
#222=MANIFOLD_SOLID_BREP('Body1',#1332);
#223=MANIFOLD_SOLID_BREP('Body1',#1333);
#224=MANIFOLD_SOLID_BREP('Body1',#1334);
#225=MANIFOLD_SOLID_BREP('Body1',#1335);
#226=MANIFOLD_SOLID_BREP('Body1',#1336);
#227=MANIFOLD_SOLID_BREP('Body1',#1337);
#228=MANIFOLD_SOLID_BREP('Body1',#1338);
#229=FACE_BOUND('',#387,.T.);
#230=FACE_BOUND('',#389,.T.);
#231=FACE_BOUND('',#397,.T.);
#232=FACE_BOUND('',#398,.T.);
#233=FACE_BOUND('',#399,.T.);
#234=FACE_BOUND('',#400,.T.);
#235=FACE_BOUND('',#401,.T.);
#236=FACE_BOUND('',#403,.T.);
#237=FACE_BOUND('',#404,.T.);
#238=FACE_BOUND('',#405,.T.);
#239=FACE_BOUND('',#406,.T.);
#240=FACE_BOUND('',#407,.T.);
#241=FACE_BOUND('',#415,.T.);
#242=FACE_BOUND('',#416,.T.);
#243=FACE_BOUND('',#417,.T.);
#244=FACE_BOUND('',#418,.T.);
#245=FACE_BOUND('',#419,.T.);
#246=FACE_BOUND('',#421,.T.);
#247=FACE_BOUND('',#422,.T.);
#248=FACE_BOUND('',#423,.T.);
#249=FACE_BOUND('',#424,.T.);
#250=FACE_BOUND('',#425,.T.);
#251=FACE_BOUND('',#433,.T.);
#252=FACE_BOUND('',#434,.T.);
#253=FACE_BOUND('',#435,.T.);
#254=FACE_BOUND('',#436,.T.);
#255=FACE_BOUND('',#437,.T.);
#256=FACE_BOUND('',#439,.T.);
#257=FACE_BOUND('',#440,.T.);
#258=FACE_BOUND('',#441,.T.);
#259=FACE_BOUND('',#442,.T.);
#260=FACE_BOUND('',#443,.T.);
#261=FACE_BOUND('',#451,.T.);
#262=FACE_BOUND('',#452,.T.);
#263=FACE_BOUND('',#453,.T.);
#264=FACE_BOUND('',#454,.T.);
#265=FACE_BOUND('',#455,.T.);
#266=FACE_BOUND('',#457,.T.);
#267=FACE_BOUND('',#458,.T.);
#268=FACE_BOUND('',#459,.T.);
#269=FACE_BOUND('',#460,.T.);
#270=FACE_BOUND('',#461,.T.);
#271=FACE_BOUND('',#465,.T.);
#272=FACE_BOUND('',#467,.T.);
#273=FACE_BOUND('',#471,.T.);
#274=FACE_BOUND('',#473,.T.);
#275=FACE_BOUND('',#486,.T.);
#276=FACE_BOUND('',#490,.T.);
#277=FACE_BOUND('',#492,.T.);
#278=FACE_BOUND('',#503,.T.);
#279=FACE_BOUND('',#505,.T.);
#280=PLANE('',#1458);
#281=PLANE('',#1459);
#282=PLANE('',#1479);
#283=PLANE('',#1480);
#284=PLANE('',#1500);
#285=PLANE('',#1501);
#286=PLANE('',#1521);
#287=PLANE('',#1522);
#288=PLANE('',#1542);
#289=PLANE('',#1543);
#290=PLANE('',#1551);
#291=PLANE('',#1552);
#292=PLANE('',#1560);
#293=PLANE('',#1561);
#294=PLANE('',#1568);
#295=PLANE('',#1571);
#296=PLANE('',#1572);
#297=PLANE('',#1573);
#298=PLANE('',#1574);
#299=PLANE('',#1575);
#300=PLANE('',#1576);
#301=PLANE('',#1577);
#302=PLANE('',#1578);
#303=PLANE('',#1586);
#304=PLANE('',#1587);
#305=PLANE('',#1593);
#306=PLANE('',#1594);
#307=PLANE('',#1595);
#308=PLANE('',#1599);
#309=PLANE('',#1600);
#310=PLANE('',#1601);
#311=PLANE('',#1602);
#312=PLANE('',#1603);
#313=FACE_OUTER_BOUND('',#384,.T.);
#314=FACE_OUTER_BOUND('',#385,.T.);
#315=FACE_OUTER_BOUND('',#386,.T.);
#316=FACE_OUTER_BOUND('',#388,.T.);
#317=FACE_OUTER_BOUND('',#390,.T.);
#318=FACE_OUTER_BOUND('',#391,.T.);
#319=FACE_OUTER_BOUND('',#392,.T.);
#320=FACE_OUTER_BOUND('',#393,.T.);
#321=FACE_OUTER_BOUND('',#394,.T.);
#322=FACE_OUTER_BOUND('',#395,.T.);
#323=FACE_OUTER_BOUND('',#396,.T.);
#324=FACE_OUTER_BOUND('',#402,.T.);
#325=FACE_OUTER_BOUND('',#408,.T.);
#326=FACE_OUTER_BOUND('',#409,.T.);
#327=FACE_OUTER_BOUND('',#410,.T.);
#328=FACE_OUTER_BOUND('',#411,.T.);
#329=FACE_OUTER_BOUND('',#412,.T.);
#330=FACE_OUTER_BOUND('',#413,.T.);
#331=FACE_OUTER_BOUND('',#414,.T.);
#332=FACE_OUTER_BOUND('',#420,.T.);
#333=FACE_OUTER_BOUND('',#426,.T.);
#334=FACE_OUTER_BOUND('',#427,.T.);
#335=FACE_OUTER_BOUND('',#428,.T.);
#336=FACE_OUTER_BOUND('',#429,.T.);
#337=FACE_OUTER_BOUND('',#430,.T.);
#338=FACE_OUTER_BOUND('',#431,.T.);
#339=FACE_OUTER_BOUND('',#432,.T.);
#340=FACE_OUTER_BOUND('',#438,.T.);
#341=FACE_OUTER_BOUND('',#444,.T.);
#342=FACE_OUTER_BOUND('',#445,.T.);
#343=FACE_OUTER_BOUND('',#446,.T.);
#344=FACE_OUTER_BOUND('',#447,.T.);
#345=FACE_OUTER_BOUND('',#448,.T.);
#346=FACE_OUTER_BOUND('',#449,.T.);
#347=FACE_OUTER_BOUND('',#450,.T.);
#348=FACE_OUTER_BOUND('',#456,.T.);
#349=FACE_OUTER_BOUND('',#462,.T.);
#350=FACE_OUTER_BOUND('',#463,.T.);
#351=FACE_OUTER_BOUND('',#464,.T.);
#352=FACE_OUTER_BOUND('',#466,.T.);
#353=FACE_OUTER_BOUND('',#468,.T.);
#354=FACE_OUTER_BOUND('',#469,.T.);
#355=FACE_OUTER_BOUND('',#470,.T.);
#356=FACE_OUTER_BOUND('',#472,.T.);
#357=FACE_OUTER_BOUND('',#474,.T.);
#358=FACE_OUTER_BOUND('',#475,.T.);
#359=FACE_OUTER_BOUND('',#476,.T.);
#360=FACE_OUTER_BOUND('',#477,.T.);
#361=FACE_OUTER_BOUND('',#478,.T.);
#362=FACE_OUTER_BOUND('',#479,.T.);
#363=FACE_OUTER_BOUND('',#480,.T.);
#364=FACE_OUTER_BOUND('',#481,.T.);
#365=FACE_OUTER_BOUND('',#482,.T.);
#366=FACE_OUTER_BOUND('',#483,.T.);
#367=FACE_OUTER_BOUND('',#484,.T.);
#368=FACE_OUTER_BOUND('',#485,.T.);
#369=FACE_OUTER_BOUND('',#487,.T.);
#370=FACE_OUTER_BOUND('',#488,.T.);
#371=FACE_OUTER_BOUND('',#489,.T.);
#372=FACE_OUTER_BOUND('',#491,.T.);
#373=FACE_OUTER_BOUND('',#493,.T.);
#374=FACE_OUTER_BOUND('',#494,.T.);
#375=FACE_OUTER_BOUND('',#495,.T.);
#376=FACE_OUTER_BOUND('',#496,.T.);
#377=FACE_OUTER_BOUND('',#497,.T.);
#378=FACE_OUTER_BOUND('',#498,.T.);
#379=FACE_OUTER_BOUND('',#499,.T.);
#380=FACE_OUTER_BOUND('',#500,.T.);
#381=FACE_OUTER_BOUND('',#501,.T.);
#382=FACE_OUTER_BOUND('',#502,.T.);
#383=FACE_OUTER_BOUND('',#504,.T.);
#384=EDGE_LOOP('',(#932,#933,#934,#935));
#385=EDGE_LOOP('',(#936,#937,#938,#939));
#386=EDGE_LOOP('',(#940));
#387=EDGE_LOOP('',(#941));
#388=EDGE_LOOP('',(#942));
#389=EDGE_LOOP('',(#943));
#390=EDGE_LOOP('',(#944,#945,#946,#947));
#391=EDGE_LOOP('',(#948,#949,#950,#951));
#392=EDGE_LOOP('',(#952,#953,#954,#955));
#393=EDGE_LOOP('',(#956,#957,#958,#959));
#394=EDGE_LOOP('',(#960,#961,#962,#963));
#395=EDGE_LOOP('',(#964,#965,#966,#967));
#396=EDGE_LOOP('',(#968));
#397=EDGE_LOOP('',(#969));
#398=EDGE_LOOP('',(#970));
#399=EDGE_LOOP('',(#971));
#400=EDGE_LOOP('',(#972));
#401=EDGE_LOOP('',(#973));
#402=EDGE_LOOP('',(#974));
#403=EDGE_LOOP('',(#975));
#404=EDGE_LOOP('',(#976));
#405=EDGE_LOOP('',(#977));
#406=EDGE_LOOP('',(#978));
#407=EDGE_LOOP('',(#979));
#408=EDGE_LOOP('',(#980,#981,#982,#983));
#409=EDGE_LOOP('',(#984,#985,#986,#987));
#410=EDGE_LOOP('',(#988,#989,#990,#991));
#411=EDGE_LOOP('',(#992,#993,#994,#995));
#412=EDGE_LOOP('',(#996,#997,#998,#999));
#413=EDGE_LOOP('',(#1000,#1001,#1002,#1003));
#414=EDGE_LOOP('',(#1004));
#415=EDGE_LOOP('',(#1005));
#416=EDGE_LOOP('',(#1006));
#417=EDGE_LOOP('',(#1007));
#418=EDGE_LOOP('',(#1008));
#419=EDGE_LOOP('',(#1009));
#420=EDGE_LOOP('',(#1010));
#421=EDGE_LOOP('',(#1011));
#422=EDGE_LOOP('',(#1012));
#423=EDGE_LOOP('',(#1013));
#424=EDGE_LOOP('',(#1014));
#425=EDGE_LOOP('',(#1015));
#426=EDGE_LOOP('',(#1016,#1017,#1018,#1019));
#427=EDGE_LOOP('',(#1020,#1021,#1022,#1023));
#428=EDGE_LOOP('',(#1024,#1025,#1026,#1027));
#429=EDGE_LOOP('',(#1028,#1029,#1030,#1031));
#430=EDGE_LOOP('',(#1032,#1033,#1034,#1035));
#431=EDGE_LOOP('',(#1036,#1037,#1038,#1039));
#432=EDGE_LOOP('',(#1040));
#433=EDGE_LOOP('',(#1041));
#434=EDGE_LOOP('',(#1042));
#435=EDGE_LOOP('',(#1043));
#436=EDGE_LOOP('',(#1044));
#437=EDGE_LOOP('',(#1045));
#438=EDGE_LOOP('',(#1046));
#439=EDGE_LOOP('',(#1047));
#440=EDGE_LOOP('',(#1048));
#441=EDGE_LOOP('',(#1049));
#442=EDGE_LOOP('',(#1050));
#443=EDGE_LOOP('',(#1051));
#444=EDGE_LOOP('',(#1052,#1053,#1054,#1055));
#445=EDGE_LOOP('',(#1056,#1057,#1058,#1059));
#446=EDGE_LOOP('',(#1060,#1061,#1062,#1063));
#447=EDGE_LOOP('',(#1064,#1065,#1066,#1067));
#448=EDGE_LOOP('',(#1068,#1069,#1070,#1071));
#449=EDGE_LOOP('',(#1072,#1073,#1074,#1075));
#450=EDGE_LOOP('',(#1076));
#451=EDGE_LOOP('',(#1077));
#452=EDGE_LOOP('',(#1078));
#453=EDGE_LOOP('',(#1079));
#454=EDGE_LOOP('',(#1080));
#455=EDGE_LOOP('',(#1081));
#456=EDGE_LOOP('',(#1082));
#457=EDGE_LOOP('',(#1083));
#458=EDGE_LOOP('',(#1084));
#459=EDGE_LOOP('',(#1085));
#460=EDGE_LOOP('',(#1086));
#461=EDGE_LOOP('',(#1087));
#462=EDGE_LOOP('',(#1088,#1089,#1090,#1091));
#463=EDGE_LOOP('',(#1092,#1093,#1094,#1095));
#464=EDGE_LOOP('',(#1096));
#465=EDGE_LOOP('',(#1097));
#466=EDGE_LOOP('',(#1098));
#467=EDGE_LOOP('',(#1099));
#468=EDGE_LOOP('',(#1100,#1101,#1102,#1103));
#469=EDGE_LOOP('',(#1104,#1105,#1106,#1107));
#470=EDGE_LOOP('',(#1108));
#471=EDGE_LOOP('',(#1109));
#472=EDGE_LOOP('',(#1110));
#473=EDGE_LOOP('',(#1111));
#474=EDGE_LOOP('',(#1112,#1113,#1114,#1115));
#475=EDGE_LOOP('',(#1116,#1117,#1118,#1119));
#476=EDGE_LOOP('',(#1120));
#477=EDGE_LOOP('',(#1121,#1122,#1123,#1124,#1125,#1126,#1127,#1128,#1129));
#478=EDGE_LOOP('',(#1130,#1131,#1132,#1133));
#479=EDGE_LOOP('',(#1134,#1135,#1136,#1137));
#480=EDGE_LOOP('',(#1138,#1139,#1140,#1141));
#481=EDGE_LOOP('',(#1142,#1143,#1144,#1145));
#482=EDGE_LOOP('',(#1146,#1147,#1148,#1149));
#483=EDGE_LOOP('',(#1150,#1151,#1152,#1153));
#484=EDGE_LOOP('',(#1154));
#485=EDGE_LOOP('',(#1155,#1156,#1157,#1158,#1159,#1160));
#486=EDGE_LOOP('',(#1161));
#487=EDGE_LOOP('',(#1162,#1163,#1164,#1165));
#488=EDGE_LOOP('',(#1166,#1167,#1168,#1169));
#489=EDGE_LOOP('',(#1170));
#490=EDGE_LOOP('',(#1171));
#491=EDGE_LOOP('',(#1172));
#492=EDGE_LOOP('',(#1173));
#493=EDGE_LOOP('',(#1174,#1175,#1176,#1177,#1178,#1179,#1180,#1181,#1182));
#494=EDGE_LOOP('',(#1183,#1184,#1185,#1186,#1187,#1188,#1189,#1190,#1191));
#495=EDGE_LOOP('',(#1192,#1193,#1194,#1195));
#496=EDGE_LOOP('',(#1196,#1197,#1198,#1199));
#497=EDGE_LOOP('',(#1200,#1201,#1202,#1203));
#498=EDGE_LOOP('',(#1204,#1205,#1206,#1207));
#499=EDGE_LOOP('',(#1208,#1209,#1210,#1211));
#500=EDGE_LOOP('',(#1212,#1213,#1214,#1215));
#501=EDGE_LOOP('',(#1216,#1217,#1218,#1219));
#502=EDGE_LOOP('',(#1220));
#503=EDGE_LOOP('',(#1221));
#504=EDGE_LOOP('',(#1222));
#505=EDGE_LOOP('',(#1223));
#506=LINE('',#2091,#562);
#507=LINE('',#2097,#563);
#508=LINE('',#2106,#564);
#509=LINE('',#2112,#565);
#510=LINE('',#2118,#566);
#511=LINE('',#2124,#567);
#512=LINE('',#2130,#568);
#513=LINE('',#2136,#569);
#514=LINE('',#2145,#570);
#515=LINE('',#2151,#571);
#516=LINE('',#2157,#572);
#517=LINE('',#2163,#573);
#518=LINE('',#2169,#574);
#519=LINE('',#2175,#575);
#520=LINE('',#2184,#576);
#521=LINE('',#2190,#577);
#522=LINE('',#2196,#578);
#523=LINE('',#2202,#579);
#524=LINE('',#2208,#580);
#525=LINE('',#2214,#581);
#526=LINE('',#2223,#582);
#527=LINE('',#2229,#583);
#528=LINE('',#2235,#584);
#529=LINE('',#2241,#585);
#530=LINE('',#2247,#586);
#531=LINE('',#2253,#587);
#532=LINE('',#2262,#588);
#533=LINE('',#2268,#589);
#534=LINE('',#2277,#590);
#535=LINE('',#2283,#591);
#536=LINE('',#2292,#592);
#537=LINE('',#2297,#593);
#538=LINE('',#2303,#594);
#539=LINE('',#2329,#595);
#540=LINE('',#2331,#596);
#541=LINE('',#2332,#597);
#542=LINE('',#2335,#598);
#543=LINE('',#2336,#599);
#544=LINE('',#2339,#600);
#545=LINE('',#2340,#601);
#546=LINE('',#2343,#602);
#547=LINE('',#2344,#603);
#548=LINE('',#2347,#604);
#549=LINE('',#2348,#605);
#550=LINE('',#2350,#606);
#551=LINE('',#2358,#607);
#552=LINE('',#2364,#608);
#553=LINE('',#2380,#609);
#554=LINE('',#2401,#610);
#555=LINE('',#2426,#611);
#556=LINE('',#2427,#612);
#557=LINE('',#2429,#613);
#558=LINE('',#2431,#614);
#559=LINE('',#2436,#615);
#560=LINE('',#2439,#616);
#561=LINE('',#2441,#617);
#562=VECTOR('',#1651,0.79);
#563=VECTOR('',#1658,1.065);
#564=VECTOR('',#1671,0.44);
#565=VECTOR('',#1678,0.44);
#566=VECTOR('',#1685,0.44);
#567=VECTOR('',#1692,0.44);
#568=VECTOR('',#1699,1.065);
#569=VECTOR('',#1706,3.5);
#570=VECTOR('',#1719,0.44);
#571=VECTOR('',#1726,0.44);
#572=VECTOR('',#1733,0.44);
#573=VECTOR('',#1740,0.44);
#574=VECTOR('',#1747,1.065);
#575=VECTOR('',#1754,3.5);
#576=VECTOR('',#1767,0.44);
#577=VECTOR('',#1774,0.44);
#578=VECTOR('',#1781,0.44);
#579=VECTOR('',#1788,0.44);
#580=VECTOR('',#1795,1.065);
#581=VECTOR('',#1802,3.5);
#582=VECTOR('',#1815,0.44);
#583=VECTOR('',#1822,0.44);
#584=VECTOR('',#1829,0.44);
#585=VECTOR('',#1836,0.44);
#586=VECTOR('',#1843,1.065);
#587=VECTOR('',#1850,3.5);
#588=VECTOR('',#1863,1.065);
#589=VECTOR('',#1870,2.2);
#590=VECTOR('',#1883,1.065);
#591=VECTOR('',#1890,2.2);
#592=VECTOR('',#1903,0.4);
#593=VECTOR('',#1910,0.36);
#594=VECTOR('',#1917,0.734027674973257);
#595=VECTOR('',#1920,1.);
#596=VECTOR('',#1921,1.);
#597=VECTOR('',#1922,1.);
#598=VECTOR('',#1925,1.);
#599=VECTOR('',#1926,1.);
#600=VECTOR('',#1929,1.);
#601=VECTOR('',#1930,1.);
#602=VECTOR('',#1933,1.);
#603=VECTOR('',#1934,1.);
#604=VECTOR('',#1937,1.);
#605=VECTOR('',#1938,1.);
#606=VECTOR('',#1941,1.);
#607=VECTOR('',#1952,0.42);
#608=VECTOR('',#1959,0.8);
#609=VECTOR('',#1970,0.734027674973257);
#610=VECTOR('',#1977,0.734027674973257);
#611=VECTOR('',#1980,1.);
#612=VECTOR('',#1981,1.);
#613=VECTOR('',#1984,1.);
#614=VECTOR('',#1987,1.);
#615=VECTOR('',#1992,0.4);
#616=VECTOR('',#1997,1.);
#617=VECTOR('',#2000,1.);
#618=CIRCLE('',#1453,0.79);
#619=CIRCLE('',#1454,0.79);
#620=CIRCLE('',#1456,1.065);
#621=CIRCLE('',#1457,1.065);
#622=CIRCLE('',#1462,0.44);
#623=CIRCLE('',#1463,0.44);
#624=CIRCLE('',#1465,0.44);
#625=CIRCLE('',#1466,0.44);
#626=CIRCLE('',#1468,0.44);
#627=CIRCLE('',#1469,0.44);
#628=CIRCLE('',#1471,0.44);
#629=CIRCLE('',#1472,0.44);
#630=CIRCLE('',#1474,1.065);
#631=CIRCLE('',#1475,1.065);
#632=CIRCLE('',#1477,3.5);
#633=CIRCLE('',#1478,3.5);
#634=CIRCLE('',#1483,0.44);
#635=CIRCLE('',#1484,0.44);
#636=CIRCLE('',#1486,0.44);
#637=CIRCLE('',#1487,0.44);
#638=CIRCLE('',#1489,0.44);
#639=CIRCLE('',#1490,0.44);
#640=CIRCLE('',#1492,0.44);
#641=CIRCLE('',#1493,0.44);
#642=CIRCLE('',#1495,1.065);
#643=CIRCLE('',#1496,1.065);
#644=CIRCLE('',#1498,3.5);
#645=CIRCLE('',#1499,3.5);
#646=CIRCLE('',#1504,0.44);
#647=CIRCLE('',#1505,0.44);
#648=CIRCLE('',#1507,0.44);
#649=CIRCLE('',#1508,0.44);
#650=CIRCLE('',#1510,0.44);
#651=CIRCLE('',#1511,0.44);
#652=CIRCLE('',#1513,0.44);
#653=CIRCLE('',#1514,0.44);
#654=CIRCLE('',#1516,1.065);
#655=CIRCLE('',#1517,1.065);
#656=CIRCLE('',#1519,3.5);
#657=CIRCLE('',#1520,3.5);
#658=CIRCLE('',#1525,0.44);
#659=CIRCLE('',#1526,0.44);
#660=CIRCLE('',#1528,0.44);
#661=CIRCLE('',#1529,0.44);
#662=CIRCLE('',#1531,0.44);
#663=CIRCLE('',#1532,0.44);
#664=CIRCLE('',#1534,0.44);
#665=CIRCLE('',#1535,0.44);
#666=CIRCLE('',#1537,1.065);
#667=CIRCLE('',#1538,1.065);
#668=CIRCLE('',#1540,3.5);
#669=CIRCLE('',#1541,3.5);
#670=CIRCLE('',#1546,1.065);
#671=CIRCLE('',#1547,1.065);
#672=CIRCLE('',#1549,2.2);
#673=CIRCLE('',#1550,2.2);
#674=CIRCLE('',#1555,1.065);
#675=CIRCLE('',#1556,1.065);
#676=CIRCLE('',#1558,2.2);
#677=CIRCLE('',#1559,2.2);
#678=CIRCLE('',#1564,0.3933);
#679=CIRCLE('',#1565,0.3933);
#680=CIRCLE('',#1567,0.32);
#681=CIRCLE('',#1570,0.6175);
#682=CIRCLE('',#1581,0.42);
#683=CIRCLE('',#1582,0.42);
#684=CIRCLE('',#1584,0.8);
#685=CIRCLE('',#1585,0.8);
#686=CIRCLE('',#1590,0.6175);
#687=CIRCLE('',#1592,0.6175);
#688=CIRCLE('',#1597,0.338975);
#689=CIRCLE('',#1598,0.338975);
#690=VERTEX_POINT('',#2088);
#691=VERTEX_POINT('',#2090);
#692=VERTEX_POINT('',#2094);
#693=VERTEX_POINT('',#2096);
#694=VERTEX_POINT('',#2103);
#695=VERTEX_POINT('',#2105);
#696=VERTEX_POINT('',#2109);
#697=VERTEX_POINT('',#2111);
#698=VERTEX_POINT('',#2115);
#699=VERTEX_POINT('',#2117);
#700=VERTEX_POINT('',#2121);
#701=VERTEX_POINT('',#2123);
#702=VERTEX_POINT('',#2127);
#703=VERTEX_POINT('',#2129);
#704=VERTEX_POINT('',#2133);
#705=VERTEX_POINT('',#2135);
#706=VERTEX_POINT('',#2142);
#707=VERTEX_POINT('',#2144);
#708=VERTEX_POINT('',#2148);
#709=VERTEX_POINT('',#2150);
#710=VERTEX_POINT('',#2154);
#711=VERTEX_POINT('',#2156);
#712=VERTEX_POINT('',#2160);
#713=VERTEX_POINT('',#2162);
#714=VERTEX_POINT('',#2166);
#715=VERTEX_POINT('',#2168);
#716=VERTEX_POINT('',#2172);
#717=VERTEX_POINT('',#2174);
#718=VERTEX_POINT('',#2181);
#719=VERTEX_POINT('',#2183);
#720=VERTEX_POINT('',#2187);
#721=VERTEX_POINT('',#2189);
#722=VERTEX_POINT('',#2193);
#723=VERTEX_POINT('',#2195);
#724=VERTEX_POINT('',#2199);
#725=VERTEX_POINT('',#2201);
#726=VERTEX_POINT('',#2205);
#727=VERTEX_POINT('',#2207);
#728=VERTEX_POINT('',#2211);
#729=VERTEX_POINT('',#2213);
#730=VERTEX_POINT('',#2220);
#731=VERTEX_POINT('',#2222);
#732=VERTEX_POINT('',#2226);
#733=VERTEX_POINT('',#2228);
#734=VERTEX_POINT('',#2232);
#735=VERTEX_POINT('',#2234);
#736=VERTEX_POINT('',#2238);
#737=VERTEX_POINT('',#2240);
#738=VERTEX_POINT('',#2244);
#739=VERTEX_POINT('',#2246);
#740=VERTEX_POINT('',#2250);
#741=VERTEX_POINT('',#2252);
#742=VERTEX_POINT('',#2259);
#743=VERTEX_POINT('',#2261);
#744=VERTEX_POINT('',#2265);
#745=VERTEX_POINT('',#2267);
#746=VERTEX_POINT('',#2274);
#747=VERTEX_POINT('',#2276);
#748=VERTEX_POINT('',#2280);
#749=VERTEX_POINT('',#2282);
#750=VERTEX_POINT('',#2289);
#751=VERTEX_POINT('',#2291);
#752=VERTEX_POINT('',#2295);
#753=VERTEX_POINT('',#2300);
#754=VERTEX_POINT('',#2302);
#755=VERTEX_POINT('',#2304);
#756=VERTEX_POINT('',#2308);
#757=VERTEX_POINT('',#2312);
#758=VERTEX_POINT('',#2316);
#759=VERTEX_POINT('',#2320);
#760=VERTEX_POINT('',#2328);
#761=VERTEX_POINT('',#2330);
#762=VERTEX_POINT('',#2334);
#763=VERTEX_POINT('',#2338);
#764=VERTEX_POINT('',#2342);
#765=VERTEX_POINT('',#2346);
#766=VERTEX_POINT('',#2355);
#767=VERTEX_POINT('',#2357);
#768=VERTEX_POINT('',#2361);
#769=VERTEX_POINT('',#2363);
#770=VERTEX_POINT('',#2370);
#771=VERTEX_POINT('',#2371);
#772=VERTEX_POINT('',#2375);
#773=VERTEX_POINT('',#2379);
#774=VERTEX_POINT('',#2382);
#775=VERTEX_POINT('',#2386);
#776=VERTEX_POINT('',#2390);
#777=VERTEX_POINT('',#2398);
#778=VERTEX_POINT('',#2400);
#779=VERTEX_POINT('',#2402);
#780=VERTEX_POINT('',#2406);
#781=VERTEX_POINT('',#2410);
#782=VERTEX_POINT('',#2414);
#783=VERTEX_POINT('',#2418);
#784=VERTEX_POINT('',#2433);
#785=VERTEX_POINT('',#2435);
#786=EDGE_CURVE('',#690,#690,#618,.T.);
#787=EDGE_CURVE('',#690,#691,#506,.T.);
#788=EDGE_CURVE('',#691,#691,#619,.T.);
#789=EDGE_CURVE('',#692,#692,#620,.T.);
#790=EDGE_CURVE('',#692,#693,#507,.T.);
#791=EDGE_CURVE('',#693,#693,#621,.T.);
#792=EDGE_CURVE('',#694,#694,#622,.T.);
#793=EDGE_CURVE('',#694,#695,#508,.T.);
#794=EDGE_CURVE('',#695,#695,#623,.T.);
#795=EDGE_CURVE('',#696,#696,#624,.T.);
#796=EDGE_CURVE('',#696,#697,#509,.T.);
#797=EDGE_CURVE('',#697,#697,#625,.T.);
#798=EDGE_CURVE('',#698,#698,#626,.T.);
#799=EDGE_CURVE('',#698,#699,#510,.T.);
#800=EDGE_CURVE('',#699,#699,#627,.T.);
#801=EDGE_CURVE('',#700,#700,#628,.T.);
#802=EDGE_CURVE('',#700,#701,#511,.T.);
#803=EDGE_CURVE('',#701,#701,#629,.T.);
#804=EDGE_CURVE('',#702,#702,#630,.T.);
#805=EDGE_CURVE('',#702,#703,#512,.T.);
#806=EDGE_CURVE('',#703,#703,#631,.T.);
#807=EDGE_CURVE('',#704,#704,#632,.T.);
#808=EDGE_CURVE('',#704,#705,#513,.T.);
#809=EDGE_CURVE('',#705,#705,#633,.T.);
#810=EDGE_CURVE('',#706,#706,#634,.T.);
#811=EDGE_CURVE('',#706,#707,#514,.T.);
#812=EDGE_CURVE('',#707,#707,#635,.T.);
#813=EDGE_CURVE('',#708,#708,#636,.T.);
#814=EDGE_CURVE('',#708,#709,#515,.T.);
#815=EDGE_CURVE('',#709,#709,#637,.T.);
#816=EDGE_CURVE('',#710,#710,#638,.T.);
#817=EDGE_CURVE('',#710,#711,#516,.T.);
#818=EDGE_CURVE('',#711,#711,#639,.T.);
#819=EDGE_CURVE('',#712,#712,#640,.T.);
#820=EDGE_CURVE('',#712,#713,#517,.T.);
#821=EDGE_CURVE('',#713,#713,#641,.T.);
#822=EDGE_CURVE('',#714,#714,#642,.T.);
#823=EDGE_CURVE('',#714,#715,#518,.T.);
#824=EDGE_CURVE('',#715,#715,#643,.T.);
#825=EDGE_CURVE('',#716,#716,#644,.T.);
#826=EDGE_CURVE('',#716,#717,#519,.T.);
#827=EDGE_CURVE('',#717,#717,#645,.T.);
#828=EDGE_CURVE('',#718,#718,#646,.T.);
#829=EDGE_CURVE('',#718,#719,#520,.T.);
#830=EDGE_CURVE('',#719,#719,#647,.T.);
#831=EDGE_CURVE('',#720,#720,#648,.T.);
#832=EDGE_CURVE('',#720,#721,#521,.T.);
#833=EDGE_CURVE('',#721,#721,#649,.T.);
#834=EDGE_CURVE('',#722,#722,#650,.T.);
#835=EDGE_CURVE('',#722,#723,#522,.T.);
#836=EDGE_CURVE('',#723,#723,#651,.T.);
#837=EDGE_CURVE('',#724,#724,#652,.T.);
#838=EDGE_CURVE('',#724,#725,#523,.T.);
#839=EDGE_CURVE('',#725,#725,#653,.T.);
#840=EDGE_CURVE('',#726,#726,#654,.T.);
#841=EDGE_CURVE('',#726,#727,#524,.T.);
#842=EDGE_CURVE('',#727,#727,#655,.T.);
#843=EDGE_CURVE('',#728,#728,#656,.T.);
#844=EDGE_CURVE('',#728,#729,#525,.T.);
#845=EDGE_CURVE('',#729,#729,#657,.T.);
#846=EDGE_CURVE('',#730,#730,#658,.T.);
#847=EDGE_CURVE('',#730,#731,#526,.T.);
#848=EDGE_CURVE('',#731,#731,#659,.T.);
#849=EDGE_CURVE('',#732,#732,#660,.T.);
#850=EDGE_CURVE('',#732,#733,#527,.T.);
#851=EDGE_CURVE('',#733,#733,#661,.T.);
#852=EDGE_CURVE('',#734,#734,#662,.T.);
#853=EDGE_CURVE('',#734,#735,#528,.T.);
#854=EDGE_CURVE('',#735,#735,#663,.T.);
#855=EDGE_CURVE('',#736,#736,#664,.T.);
#856=EDGE_CURVE('',#736,#737,#529,.T.);
#857=EDGE_CURVE('',#737,#737,#665,.T.);
#858=EDGE_CURVE('',#738,#738,#666,.T.);
#859=EDGE_CURVE('',#738,#739,#530,.T.);
#860=EDGE_CURVE('',#739,#739,#667,.T.);
#861=EDGE_CURVE('',#740,#740,#668,.T.);
#862=EDGE_CURVE('',#740,#741,#531,.T.);
#863=EDGE_CURVE('',#741,#741,#669,.T.);
#864=EDGE_CURVE('',#742,#742,#670,.T.);
#865=EDGE_CURVE('',#742,#743,#532,.T.);
#866=EDGE_CURVE('',#743,#743,#671,.T.);
#867=EDGE_CURVE('',#744,#744,#672,.T.);
#868=EDGE_CURVE('',#744,#745,#533,.T.);
#869=EDGE_CURVE('',#745,#745,#673,.T.);
#870=EDGE_CURVE('',#746,#746,#674,.T.);
#871=EDGE_CURVE('',#746,#747,#534,.T.);
#872=EDGE_CURVE('',#747,#747,#675,.T.);
#873=EDGE_CURVE('',#748,#748,#676,.T.);
#874=EDGE_CURVE('',#748,#749,#535,.T.);
#875=EDGE_CURVE('',#749,#749,#677,.T.);
#876=EDGE_CURVE('',#750,#750,#678,.F.);
#877=EDGE_CURVE('',#750,#751,#536,.T.);
#878=EDGE_CURVE('',#751,#751,#679,.F.);
#879=EDGE_CURVE('',#752,#752,#680,.T.);
#880=EDGE_CURVE('',#752,#750,#537,.T.);
#881=EDGE_CURVE('',#753,#753,#681,.T.);
#882=EDGE_CURVE('',#753,#754,#538,.T.);
#883=EDGE_CURVE('',#755,#754,#167,.T.);
#884=EDGE_CURVE('',#756,#755,#168,.T.);
#885=EDGE_CURVE('',#757,#756,#169,.T.);
#886=EDGE_CURVE('',#758,#757,#170,.T.);
#887=EDGE_CURVE('',#759,#758,#171,.T.);
#888=EDGE_CURVE('',#754,#759,#172,.T.);
#889=EDGE_CURVE('',#760,#758,#539,.T.);
#890=EDGE_CURVE('',#760,#761,#540,.T.);
#891=EDGE_CURVE('',#761,#759,#541,.T.);
#892=EDGE_CURVE('',#762,#757,#542,.T.);
#893=EDGE_CURVE('',#762,#760,#543,.T.);
#894=EDGE_CURVE('',#763,#756,#544,.T.);
#895=EDGE_CURVE('',#763,#762,#545,.T.);
#896=EDGE_CURVE('',#764,#755,#546,.T.);
#897=EDGE_CURVE('',#764,#763,#547,.T.);
#898=EDGE_CURVE('',#765,#754,#548,.T.);
#899=EDGE_CURVE('',#765,#764,#549,.T.);
#900=EDGE_CURVE('',#761,#765,#550,.T.);
#901=EDGE_CURVE('',#766,#766,#682,.T.);
#902=EDGE_CURVE('',#766,#767,#551,.T.);
#903=EDGE_CURVE('',#767,#767,#683,.T.);
#904=EDGE_CURVE('',#768,#768,#684,.T.);
#905=EDGE_CURVE('',#768,#769,#552,.T.);
#906=EDGE_CURVE('',#769,#769,#685,.T.);
#907=EDGE_CURVE('',#770,#771,#173,.T.);
#908=EDGE_CURVE('',#772,#770,#174,.T.);
#909=EDGE_CURVE('',#772,#773,#553,.T.);
#910=EDGE_CURVE('',#773,#773,#686,.T.);
#911=EDGE_CURVE('',#774,#772,#175,.T.);
#912=EDGE_CURVE('',#775,#774,#176,.T.);
#913=EDGE_CURVE('',#776,#775,#177,.T.);
#914=EDGE_CURVE('',#771,#776,#178,.T.);
#915=EDGE_CURVE('',#777,#777,#687,.T.);
#916=EDGE_CURVE('',#777,#778,#554,.T.);
#917=EDGE_CURVE('',#779,#778,#179,.T.);
#918=EDGE_CURVE('',#780,#779,#180,.T.);
#919=EDGE_CURVE('',#781,#780,#181,.T.);
#920=EDGE_CURVE('',#782,#781,#182,.T.);
#921=EDGE_CURVE('',#783,#782,#183,.T.);
#922=EDGE_CURVE('',#778,#783,#184,.T.);
#923=EDGE_CURVE('',#774,#783,#555,.T.);
#924=EDGE_CURVE('',#775,#782,#556,.T.);
#925=EDGE_CURVE('',#772,#778,#557,.T.);
#926=EDGE_CURVE('',#770,#779,#558,.T.);
#927=EDGE_CURVE('',#784,#784,#688,.F.);
#928=EDGE_CURVE('',#784,#785,#559,.T.);
#929=EDGE_CURVE('',#785,#785,#689,.F.);
#930=EDGE_CURVE('',#771,#780,#560,.T.);
#931=EDGE_CURVE('',#776,#781,#561,.T.);
#932=ORIENTED_EDGE('',*,*,#786,.F.);
#933=ORIENTED_EDGE('',*,*,#787,.T.);
#934=ORIENTED_EDGE('',*,*,#788,.T.);
#935=ORIENTED_EDGE('',*,*,#787,.F.);
#936=ORIENTED_EDGE('',*,*,#789,.F.);
#937=ORIENTED_EDGE('',*,*,#790,.T.);
#938=ORIENTED_EDGE('',*,*,#791,.T.);
#939=ORIENTED_EDGE('',*,*,#790,.F.);
#940=ORIENTED_EDGE('',*,*,#789,.T.);
#941=ORIENTED_EDGE('',*,*,#786,.T.);
#942=ORIENTED_EDGE('',*,*,#791,.F.);
#943=ORIENTED_EDGE('',*,*,#788,.F.);
#944=ORIENTED_EDGE('',*,*,#792,.F.);
#945=ORIENTED_EDGE('',*,*,#793,.T.);
#946=ORIENTED_EDGE('',*,*,#794,.F.);
#947=ORIENTED_EDGE('',*,*,#793,.F.);
#948=ORIENTED_EDGE('',*,*,#795,.F.);
#949=ORIENTED_EDGE('',*,*,#796,.T.);
#950=ORIENTED_EDGE('',*,*,#797,.F.);
#951=ORIENTED_EDGE('',*,*,#796,.F.);
#952=ORIENTED_EDGE('',*,*,#798,.F.);
#953=ORIENTED_EDGE('',*,*,#799,.T.);
#954=ORIENTED_EDGE('',*,*,#800,.F.);
#955=ORIENTED_EDGE('',*,*,#799,.F.);
#956=ORIENTED_EDGE('',*,*,#801,.F.);
#957=ORIENTED_EDGE('',*,*,#802,.T.);
#958=ORIENTED_EDGE('',*,*,#803,.F.);
#959=ORIENTED_EDGE('',*,*,#802,.F.);
#960=ORIENTED_EDGE('',*,*,#804,.F.);
#961=ORIENTED_EDGE('',*,*,#805,.T.);
#962=ORIENTED_EDGE('',*,*,#806,.T.);
#963=ORIENTED_EDGE('',*,*,#805,.F.);
#964=ORIENTED_EDGE('',*,*,#807,.F.);
#965=ORIENTED_EDGE('',*,*,#808,.T.);
#966=ORIENTED_EDGE('',*,*,#809,.T.);
#967=ORIENTED_EDGE('',*,*,#808,.F.);
#968=ORIENTED_EDGE('',*,*,#807,.T.);
#969=ORIENTED_EDGE('',*,*,#804,.T.);
#970=ORIENTED_EDGE('',*,*,#803,.T.);
#971=ORIENTED_EDGE('',*,*,#800,.T.);
#972=ORIENTED_EDGE('',*,*,#797,.T.);
#973=ORIENTED_EDGE('',*,*,#794,.T.);
#974=ORIENTED_EDGE('',*,*,#809,.F.);
#975=ORIENTED_EDGE('',*,*,#806,.F.);
#976=ORIENTED_EDGE('',*,*,#801,.T.);
#977=ORIENTED_EDGE('',*,*,#798,.T.);
#978=ORIENTED_EDGE('',*,*,#795,.T.);
#979=ORIENTED_EDGE('',*,*,#792,.T.);
#980=ORIENTED_EDGE('',*,*,#810,.F.);
#981=ORIENTED_EDGE('',*,*,#811,.T.);
#982=ORIENTED_EDGE('',*,*,#812,.F.);
#983=ORIENTED_EDGE('',*,*,#811,.F.);
#984=ORIENTED_EDGE('',*,*,#813,.F.);
#985=ORIENTED_EDGE('',*,*,#814,.T.);
#986=ORIENTED_EDGE('',*,*,#815,.F.);
#987=ORIENTED_EDGE('',*,*,#814,.F.);
#988=ORIENTED_EDGE('',*,*,#816,.F.);
#989=ORIENTED_EDGE('',*,*,#817,.T.);
#990=ORIENTED_EDGE('',*,*,#818,.F.);
#991=ORIENTED_EDGE('',*,*,#817,.F.);
#992=ORIENTED_EDGE('',*,*,#819,.F.);
#993=ORIENTED_EDGE('',*,*,#820,.T.);
#994=ORIENTED_EDGE('',*,*,#821,.F.);
#995=ORIENTED_EDGE('',*,*,#820,.F.);
#996=ORIENTED_EDGE('',*,*,#822,.F.);
#997=ORIENTED_EDGE('',*,*,#823,.T.);
#998=ORIENTED_EDGE('',*,*,#824,.T.);
#999=ORIENTED_EDGE('',*,*,#823,.F.);
#1000=ORIENTED_EDGE('',*,*,#825,.F.);
#1001=ORIENTED_EDGE('',*,*,#826,.T.);
#1002=ORIENTED_EDGE('',*,*,#827,.T.);
#1003=ORIENTED_EDGE('',*,*,#826,.F.);
#1004=ORIENTED_EDGE('',*,*,#825,.T.);
#1005=ORIENTED_EDGE('',*,*,#822,.T.);
#1006=ORIENTED_EDGE('',*,*,#821,.T.);
#1007=ORIENTED_EDGE('',*,*,#818,.T.);
#1008=ORIENTED_EDGE('',*,*,#815,.T.);
#1009=ORIENTED_EDGE('',*,*,#812,.T.);
#1010=ORIENTED_EDGE('',*,*,#827,.F.);
#1011=ORIENTED_EDGE('',*,*,#824,.F.);
#1012=ORIENTED_EDGE('',*,*,#819,.T.);
#1013=ORIENTED_EDGE('',*,*,#816,.T.);
#1014=ORIENTED_EDGE('',*,*,#813,.T.);
#1015=ORIENTED_EDGE('',*,*,#810,.T.);
#1016=ORIENTED_EDGE('',*,*,#828,.F.);
#1017=ORIENTED_EDGE('',*,*,#829,.T.);
#1018=ORIENTED_EDGE('',*,*,#830,.F.);
#1019=ORIENTED_EDGE('',*,*,#829,.F.);
#1020=ORIENTED_EDGE('',*,*,#831,.F.);
#1021=ORIENTED_EDGE('',*,*,#832,.T.);
#1022=ORIENTED_EDGE('',*,*,#833,.F.);
#1023=ORIENTED_EDGE('',*,*,#832,.F.);
#1024=ORIENTED_EDGE('',*,*,#834,.F.);
#1025=ORIENTED_EDGE('',*,*,#835,.T.);
#1026=ORIENTED_EDGE('',*,*,#836,.F.);
#1027=ORIENTED_EDGE('',*,*,#835,.F.);
#1028=ORIENTED_EDGE('',*,*,#837,.F.);
#1029=ORIENTED_EDGE('',*,*,#838,.T.);
#1030=ORIENTED_EDGE('',*,*,#839,.F.);
#1031=ORIENTED_EDGE('',*,*,#838,.F.);
#1032=ORIENTED_EDGE('',*,*,#840,.F.);
#1033=ORIENTED_EDGE('',*,*,#841,.T.);
#1034=ORIENTED_EDGE('',*,*,#842,.T.);
#1035=ORIENTED_EDGE('',*,*,#841,.F.);
#1036=ORIENTED_EDGE('',*,*,#843,.F.);
#1037=ORIENTED_EDGE('',*,*,#844,.T.);
#1038=ORIENTED_EDGE('',*,*,#845,.T.);
#1039=ORIENTED_EDGE('',*,*,#844,.F.);
#1040=ORIENTED_EDGE('',*,*,#843,.T.);
#1041=ORIENTED_EDGE('',*,*,#840,.T.);
#1042=ORIENTED_EDGE('',*,*,#839,.T.);
#1043=ORIENTED_EDGE('',*,*,#836,.T.);
#1044=ORIENTED_EDGE('',*,*,#833,.T.);
#1045=ORIENTED_EDGE('',*,*,#830,.T.);
#1046=ORIENTED_EDGE('',*,*,#845,.F.);
#1047=ORIENTED_EDGE('',*,*,#842,.F.);
#1048=ORIENTED_EDGE('',*,*,#837,.T.);
#1049=ORIENTED_EDGE('',*,*,#834,.T.);
#1050=ORIENTED_EDGE('',*,*,#831,.T.);
#1051=ORIENTED_EDGE('',*,*,#828,.T.);
#1052=ORIENTED_EDGE('',*,*,#846,.F.);
#1053=ORIENTED_EDGE('',*,*,#847,.T.);
#1054=ORIENTED_EDGE('',*,*,#848,.F.);
#1055=ORIENTED_EDGE('',*,*,#847,.F.);
#1056=ORIENTED_EDGE('',*,*,#849,.F.);
#1057=ORIENTED_EDGE('',*,*,#850,.T.);
#1058=ORIENTED_EDGE('',*,*,#851,.F.);
#1059=ORIENTED_EDGE('',*,*,#850,.F.);
#1060=ORIENTED_EDGE('',*,*,#852,.F.);
#1061=ORIENTED_EDGE('',*,*,#853,.T.);
#1062=ORIENTED_EDGE('',*,*,#854,.F.);
#1063=ORIENTED_EDGE('',*,*,#853,.F.);
#1064=ORIENTED_EDGE('',*,*,#855,.F.);
#1065=ORIENTED_EDGE('',*,*,#856,.T.);
#1066=ORIENTED_EDGE('',*,*,#857,.F.);
#1067=ORIENTED_EDGE('',*,*,#856,.F.);
#1068=ORIENTED_EDGE('',*,*,#858,.F.);
#1069=ORIENTED_EDGE('',*,*,#859,.T.);
#1070=ORIENTED_EDGE('',*,*,#860,.T.);
#1071=ORIENTED_EDGE('',*,*,#859,.F.);
#1072=ORIENTED_EDGE('',*,*,#861,.F.);
#1073=ORIENTED_EDGE('',*,*,#862,.T.);
#1074=ORIENTED_EDGE('',*,*,#863,.T.);
#1075=ORIENTED_EDGE('',*,*,#862,.F.);
#1076=ORIENTED_EDGE('',*,*,#861,.T.);
#1077=ORIENTED_EDGE('',*,*,#858,.T.);
#1078=ORIENTED_EDGE('',*,*,#857,.T.);
#1079=ORIENTED_EDGE('',*,*,#854,.T.);
#1080=ORIENTED_EDGE('',*,*,#851,.T.);
#1081=ORIENTED_EDGE('',*,*,#848,.T.);
#1082=ORIENTED_EDGE('',*,*,#863,.F.);
#1083=ORIENTED_EDGE('',*,*,#860,.F.);
#1084=ORIENTED_EDGE('',*,*,#855,.T.);
#1085=ORIENTED_EDGE('',*,*,#852,.T.);
#1086=ORIENTED_EDGE('',*,*,#849,.T.);
#1087=ORIENTED_EDGE('',*,*,#846,.T.);
#1088=ORIENTED_EDGE('',*,*,#864,.F.);
#1089=ORIENTED_EDGE('',*,*,#865,.T.);
#1090=ORIENTED_EDGE('',*,*,#866,.T.);
#1091=ORIENTED_EDGE('',*,*,#865,.F.);
#1092=ORIENTED_EDGE('',*,*,#867,.F.);
#1093=ORIENTED_EDGE('',*,*,#868,.T.);
#1094=ORIENTED_EDGE('',*,*,#869,.T.);
#1095=ORIENTED_EDGE('',*,*,#868,.F.);
#1096=ORIENTED_EDGE('',*,*,#867,.T.);
#1097=ORIENTED_EDGE('',*,*,#864,.T.);
#1098=ORIENTED_EDGE('',*,*,#869,.F.);
#1099=ORIENTED_EDGE('',*,*,#866,.F.);
#1100=ORIENTED_EDGE('',*,*,#870,.F.);
#1101=ORIENTED_EDGE('',*,*,#871,.T.);
#1102=ORIENTED_EDGE('',*,*,#872,.T.);
#1103=ORIENTED_EDGE('',*,*,#871,.F.);
#1104=ORIENTED_EDGE('',*,*,#873,.F.);
#1105=ORIENTED_EDGE('',*,*,#874,.T.);
#1106=ORIENTED_EDGE('',*,*,#875,.T.);
#1107=ORIENTED_EDGE('',*,*,#874,.F.);
#1108=ORIENTED_EDGE('',*,*,#873,.T.);
#1109=ORIENTED_EDGE('',*,*,#870,.T.);
#1110=ORIENTED_EDGE('',*,*,#875,.F.);
#1111=ORIENTED_EDGE('',*,*,#872,.F.);
#1112=ORIENTED_EDGE('',*,*,#876,.F.);
#1113=ORIENTED_EDGE('',*,*,#877,.T.);
#1114=ORIENTED_EDGE('',*,*,#878,.F.);
#1115=ORIENTED_EDGE('',*,*,#877,.F.);
#1116=ORIENTED_EDGE('',*,*,#879,.F.);
#1117=ORIENTED_EDGE('',*,*,#880,.T.);
#1118=ORIENTED_EDGE('',*,*,#876,.T.);
#1119=ORIENTED_EDGE('',*,*,#880,.F.);
#1120=ORIENTED_EDGE('',*,*,#879,.T.);
#1121=ORIENTED_EDGE('',*,*,#881,.F.);
#1122=ORIENTED_EDGE('',*,*,#882,.T.);
#1123=ORIENTED_EDGE('',*,*,#883,.F.);
#1124=ORIENTED_EDGE('',*,*,#884,.F.);
#1125=ORIENTED_EDGE('',*,*,#885,.F.);
#1126=ORIENTED_EDGE('',*,*,#886,.F.);
#1127=ORIENTED_EDGE('',*,*,#887,.F.);
#1128=ORIENTED_EDGE('',*,*,#888,.F.);
#1129=ORIENTED_EDGE('',*,*,#882,.F.);
#1130=ORIENTED_EDGE('',*,*,#887,.T.);
#1131=ORIENTED_EDGE('',*,*,#889,.F.);
#1132=ORIENTED_EDGE('',*,*,#890,.T.);
#1133=ORIENTED_EDGE('',*,*,#891,.T.);
#1134=ORIENTED_EDGE('',*,*,#886,.T.);
#1135=ORIENTED_EDGE('',*,*,#892,.F.);
#1136=ORIENTED_EDGE('',*,*,#893,.T.);
#1137=ORIENTED_EDGE('',*,*,#889,.T.);
#1138=ORIENTED_EDGE('',*,*,#885,.T.);
#1139=ORIENTED_EDGE('',*,*,#894,.F.);
#1140=ORIENTED_EDGE('',*,*,#895,.T.);
#1141=ORIENTED_EDGE('',*,*,#892,.T.);
#1142=ORIENTED_EDGE('',*,*,#884,.T.);
#1143=ORIENTED_EDGE('',*,*,#896,.F.);
#1144=ORIENTED_EDGE('',*,*,#897,.T.);
#1145=ORIENTED_EDGE('',*,*,#894,.T.);
#1146=ORIENTED_EDGE('',*,*,#883,.T.);
#1147=ORIENTED_EDGE('',*,*,#898,.F.);
#1148=ORIENTED_EDGE('',*,*,#899,.T.);
#1149=ORIENTED_EDGE('',*,*,#896,.T.);
#1150=ORIENTED_EDGE('',*,*,#888,.T.);
#1151=ORIENTED_EDGE('',*,*,#891,.F.);
#1152=ORIENTED_EDGE('',*,*,#900,.T.);
#1153=ORIENTED_EDGE('',*,*,#898,.T.);
#1154=ORIENTED_EDGE('',*,*,#881,.T.);
#1155=ORIENTED_EDGE('',*,*,#895,.F.);
#1156=ORIENTED_EDGE('',*,*,#897,.F.);
#1157=ORIENTED_EDGE('',*,*,#899,.F.);
#1158=ORIENTED_EDGE('',*,*,#900,.F.);
#1159=ORIENTED_EDGE('',*,*,#890,.F.);
#1160=ORIENTED_EDGE('',*,*,#893,.F.);
#1161=ORIENTED_EDGE('',*,*,#878,.T.);
#1162=ORIENTED_EDGE('',*,*,#901,.F.);
#1163=ORIENTED_EDGE('',*,*,#902,.T.);
#1164=ORIENTED_EDGE('',*,*,#903,.T.);
#1165=ORIENTED_EDGE('',*,*,#902,.F.);
#1166=ORIENTED_EDGE('',*,*,#904,.F.);
#1167=ORIENTED_EDGE('',*,*,#905,.T.);
#1168=ORIENTED_EDGE('',*,*,#906,.T.);
#1169=ORIENTED_EDGE('',*,*,#905,.F.);
#1170=ORIENTED_EDGE('',*,*,#904,.T.);
#1171=ORIENTED_EDGE('',*,*,#901,.T.);
#1172=ORIENTED_EDGE('',*,*,#906,.F.);
#1173=ORIENTED_EDGE('',*,*,#903,.F.);
#1174=ORIENTED_EDGE('',*,*,#907,.F.);
#1175=ORIENTED_EDGE('',*,*,#908,.F.);
#1176=ORIENTED_EDGE('',*,*,#909,.T.);
#1177=ORIENTED_EDGE('',*,*,#910,.F.);
#1178=ORIENTED_EDGE('',*,*,#909,.F.);
#1179=ORIENTED_EDGE('',*,*,#911,.F.);
#1180=ORIENTED_EDGE('',*,*,#912,.F.);
#1181=ORIENTED_EDGE('',*,*,#913,.F.);
#1182=ORIENTED_EDGE('',*,*,#914,.F.);
#1183=ORIENTED_EDGE('',*,*,#915,.F.);
#1184=ORIENTED_EDGE('',*,*,#916,.T.);
#1185=ORIENTED_EDGE('',*,*,#917,.F.);
#1186=ORIENTED_EDGE('',*,*,#918,.F.);
#1187=ORIENTED_EDGE('',*,*,#919,.F.);
#1188=ORIENTED_EDGE('',*,*,#920,.F.);
#1189=ORIENTED_EDGE('',*,*,#921,.F.);
#1190=ORIENTED_EDGE('',*,*,#922,.F.);
#1191=ORIENTED_EDGE('',*,*,#916,.F.);
#1192=ORIENTED_EDGE('',*,*,#912,.T.);
#1193=ORIENTED_EDGE('',*,*,#923,.T.);
#1194=ORIENTED_EDGE('',*,*,#921,.T.);
#1195=ORIENTED_EDGE('',*,*,#924,.F.);
#1196=ORIENTED_EDGE('',*,*,#911,.T.);
#1197=ORIENTED_EDGE('',*,*,#925,.T.);
#1198=ORIENTED_EDGE('',*,*,#922,.T.);
#1199=ORIENTED_EDGE('',*,*,#923,.F.);
#1200=ORIENTED_EDGE('',*,*,#908,.T.);
#1201=ORIENTED_EDGE('',*,*,#926,.T.);
#1202=ORIENTED_EDGE('',*,*,#917,.T.);
#1203=ORIENTED_EDGE('',*,*,#925,.F.);
#1204=ORIENTED_EDGE('',*,*,#927,.F.);
#1205=ORIENTED_EDGE('',*,*,#928,.T.);
#1206=ORIENTED_EDGE('',*,*,#929,.T.);
#1207=ORIENTED_EDGE('',*,*,#928,.F.);
#1208=ORIENTED_EDGE('',*,*,#907,.T.);
#1209=ORIENTED_EDGE('',*,*,#930,.T.);
#1210=ORIENTED_EDGE('',*,*,#918,.T.);
#1211=ORIENTED_EDGE('',*,*,#926,.F.);
#1212=ORIENTED_EDGE('',*,*,#913,.T.);
#1213=ORIENTED_EDGE('',*,*,#924,.T.);
#1214=ORIENTED_EDGE('',*,*,#920,.T.);
#1215=ORIENTED_EDGE('',*,*,#931,.F.);
#1216=ORIENTED_EDGE('',*,*,#914,.T.);
#1217=ORIENTED_EDGE('',*,*,#931,.T.);
#1218=ORIENTED_EDGE('',*,*,#919,.T.);
#1219=ORIENTED_EDGE('',*,*,#930,.F.);
#1220=ORIENTED_EDGE('',*,*,#915,.T.);
#1221=ORIENTED_EDGE('',*,*,#927,.T.);
#1222=ORIENTED_EDGE('',*,*,#910,.T.);
#1223=ORIENTED_EDGE('',*,*,#929,.F.);
#1224=CYLINDRICAL_SURFACE('',#1452,0.79);
#1225=CYLINDRICAL_SURFACE('',#1455,1.065);
#1226=CYLINDRICAL_SURFACE('',#1461,0.44);
#1227=CYLINDRICAL_SURFACE('',#1464,0.44);
#1228=CYLINDRICAL_SURFACE('',#1467,0.44);
#1229=CYLINDRICAL_SURFACE('',#1470,0.44);
#1230=CYLINDRICAL_SURFACE('',#1473,1.065);
#1231=CYLINDRICAL_SURFACE('',#1476,3.5);
#1232=CYLINDRICAL_SURFACE('',#1482,0.44);
#1233=CYLINDRICAL_SURFACE('',#1485,0.44);
#1234=CYLINDRICAL_SURFACE('',#1488,0.44);
#1235=CYLINDRICAL_SURFACE('',#1491,0.44);
#1236=CYLINDRICAL_SURFACE('',#1494,1.065);
#1237=CYLINDRICAL_SURFACE('',#1497,3.5);
#1238=CYLINDRICAL_SURFACE('',#1503,0.44);
#1239=CYLINDRICAL_SURFACE('',#1506,0.44);
#1240=CYLINDRICAL_SURFACE('',#1509,0.44);
#1241=CYLINDRICAL_SURFACE('',#1512,0.44);
#1242=CYLINDRICAL_SURFACE('',#1515,1.065);
#1243=CYLINDRICAL_SURFACE('',#1518,3.5);
#1244=CYLINDRICAL_SURFACE('',#1524,0.44);
#1245=CYLINDRICAL_SURFACE('',#1527,0.44);
#1246=CYLINDRICAL_SURFACE('',#1530,0.44);
#1247=CYLINDRICAL_SURFACE('',#1533,0.44);
#1248=CYLINDRICAL_SURFACE('',#1536,1.065);
#1249=CYLINDRICAL_SURFACE('',#1539,3.5);
#1250=CYLINDRICAL_SURFACE('',#1545,1.065);
#1251=CYLINDRICAL_SURFACE('',#1548,2.2);
#1252=CYLINDRICAL_SURFACE('',#1554,1.065);
#1253=CYLINDRICAL_SURFACE('',#1557,2.2);
#1254=CYLINDRICAL_SURFACE('',#1563,0.3933);
#1255=CYLINDRICAL_SURFACE('',#1580,0.42);
#1256=CYLINDRICAL_SURFACE('',#1583,0.8);
#1257=CYLINDRICAL_SURFACE('',#1596,0.338975);
#1258=ADVANCED_FACE('',(#313),#1224,.F.);
#1259=ADVANCED_FACE('',(#314),#1225,.T.);
#1260=ADVANCED_FACE('',(#315,#229),#280,.T.);
#1261=ADVANCED_FACE('',(#316,#230),#281,.F.);
#1262=ADVANCED_FACE('',(#317),#1226,.F.);
#1263=ADVANCED_FACE('',(#318),#1227,.F.);
#1264=ADVANCED_FACE('',(#319),#1228,.F.);
#1265=ADVANCED_FACE('',(#320),#1229,.F.);
#1266=ADVANCED_FACE('',(#321),#1230,.F.);
#1267=ADVANCED_FACE('',(#322),#1231,.T.);
#1268=ADVANCED_FACE('',(#323,#231,#232,#233,#234,#235),#282,.T.);
#1269=ADVANCED_FACE('',(#324,#236,#237,#238,#239,#240),#283,.F.);
#1270=ADVANCED_FACE('',(#325),#1232,.F.);
#1271=ADVANCED_FACE('',(#326),#1233,.F.);
#1272=ADVANCED_FACE('',(#327),#1234,.F.);
#1273=ADVANCED_FACE('',(#328),#1235,.F.);
#1274=ADVANCED_FACE('',(#329),#1236,.F.);
#1275=ADVANCED_FACE('',(#330),#1237,.T.);
#1276=ADVANCED_FACE('',(#331,#241,#242,#243,#244,#245),#284,.T.);
#1277=ADVANCED_FACE('',(#332,#246,#247,#248,#249,#250),#285,.F.);
#1278=ADVANCED_FACE('',(#333),#1238,.F.);
#1279=ADVANCED_FACE('',(#334),#1239,.F.);
#1280=ADVANCED_FACE('',(#335),#1240,.F.);
#1281=ADVANCED_FACE('',(#336),#1241,.F.);
#1282=ADVANCED_FACE('',(#337),#1242,.F.);
#1283=ADVANCED_FACE('',(#338),#1243,.T.);
#1284=ADVANCED_FACE('',(#339,#251,#252,#253,#254,#255),#286,.T.);
#1285=ADVANCED_FACE('',(#340,#256,#257,#258,#259,#260),#287,.F.);
#1286=ADVANCED_FACE('',(#341),#1244,.F.);
#1287=ADVANCED_FACE('',(#342),#1245,.F.);
#1288=ADVANCED_FACE('',(#343),#1246,.F.);
#1289=ADVANCED_FACE('',(#344),#1247,.F.);
#1290=ADVANCED_FACE('',(#345),#1248,.F.);
#1291=ADVANCED_FACE('',(#346),#1249,.T.);
#1292=ADVANCED_FACE('',(#347,#261,#262,#263,#264,#265),#288,.T.);
#1293=ADVANCED_FACE('',(#348,#266,#267,#268,#269,#270),#289,.F.);
#1294=ADVANCED_FACE('',(#349),#1250,.F.);
#1295=ADVANCED_FACE('',(#350),#1251,.T.);
#1296=ADVANCED_FACE('',(#351,#271),#290,.T.);
#1297=ADVANCED_FACE('',(#352,#272),#291,.F.);
#1298=ADVANCED_FACE('',(#353),#1252,.F.);
#1299=ADVANCED_FACE('',(#354),#1253,.T.);
#1300=ADVANCED_FACE('',(#355,#273),#292,.T.);
#1301=ADVANCED_FACE('',(#356,#274),#293,.F.);
#1302=ADVANCED_FACE('',(#357),#1254,.T.);
#1303=ADVANCED_FACE('',(#358),#185,.T.);
#1304=ADVANCED_FACE('',(#359),#294,.T.);
#1305=ADVANCED_FACE('',(#360),#186,.T.);
#1306=ADVANCED_FACE('',(#361),#295,.T.);
#1307=ADVANCED_FACE('',(#362),#296,.T.);
#1308=ADVANCED_FACE('',(#363),#297,.T.);
#1309=ADVANCED_FACE('',(#364),#298,.T.);
#1310=ADVANCED_FACE('',(#365),#299,.T.);
#1311=ADVANCED_FACE('',(#366),#300,.T.);
#1312=ADVANCED_FACE('',(#367),#301,.T.);
#1313=ADVANCED_FACE('',(#368,#275),#302,.F.);
#1314=ADVANCED_FACE('',(#369),#1255,.F.);
#1315=ADVANCED_FACE('',(#370),#1256,.T.);
#1316=ADVANCED_FACE('',(#371,#276),#303,.T.);
#1317=ADVANCED_FACE('',(#372,#277),#304,.F.);
#1318=ADVANCED_FACE('',(#373),#187,.T.);
#1319=ADVANCED_FACE('',(#374),#188,.T.);
#1320=ADVANCED_FACE('',(#375),#305,.T.);
#1321=ADVANCED_FACE('',(#376),#306,.T.);
#1322=ADVANCED_FACE('',(#377),#307,.T.);
#1323=ADVANCED_FACE('',(#378),#1257,.F.);
#1324=ADVANCED_FACE('',(#379),#308,.T.);
#1325=ADVANCED_FACE('',(#380),#309,.T.);
#1326=ADVANCED_FACE('',(#381),#310,.T.);
#1327=ADVANCED_FACE('',(#382,#278),#311,.T.);
#1328=ADVANCED_FACE('',(#383,#279),#312,.F.);
#1329=CLOSED_SHELL('',(#1258,#1259,#1260,#1261));
#1330=CLOSED_SHELL('',(#1262,#1263,#1264,#1265,#1266,#1267,#1268,#1269));
#1331=CLOSED_SHELL('',(#1270,#1271,#1272,#1273,#1274,#1275,#1276,#1277));
#1332=CLOSED_SHELL('',(#1278,#1279,#1280,#1281,#1282,#1283,#1284,#1285));
#1333=CLOSED_SHELL('',(#1286,#1287,#1288,#1289,#1290,#1291,#1292,#1293));
#1334=CLOSED_SHELL('',(#1294,#1295,#1296,#1297));
#1335=CLOSED_SHELL('',(#1298,#1299,#1300,#1301));
#1336=CLOSED_SHELL('',(#1302,#1303,#1304,#1305,#1306,#1307,#1308,#1309,
#1310,#1311,#1312,#1313));
#1337=CLOSED_SHELL('',(#1314,#1315,#1316,#1317));
#1338=CLOSED_SHELL('',(#1318,#1319,#1320,#1321,#1322,#1323,#1324,#1325,
#1326,#1327,#1328));
#1339=DERIVED_UNIT_ELEMENT(#1359,1.);
#1340=DERIVED_UNIT_ELEMENT(#2509,-3.);
#1341=DERIVED_UNIT_ELEMENT(#1359,1.);
#1342=DERIVED_UNIT_ELEMENT(#2509,-3.);
#1343=DERIVED_UNIT_ELEMENT(#1359,1.);
#1344=DERIVED_UNIT_ELEMENT(#2509,-3.);
#1345=DERIVED_UNIT_ELEMENT(#1359,1.);
#1346=DERIVED_UNIT_ELEMENT(#2509,-3.);
#1347=DERIVED_UNIT_ELEMENT(#1359,1.);
#1348=DERIVED_UNIT_ELEMENT(#2509,-3.);
#1349=DERIVED_UNIT_ELEMENT(#1359,1.);
#1350=DERIVED_UNIT_ELEMENT(#2509,-3.);
#1351=DERIVED_UNIT_ELEMENT(#1359,1.);
#1352=DERIVED_UNIT_ELEMENT(#2509,-3.);
#1353=DERIVED_UNIT_ELEMENT(#1359,1.);
#1354=DERIVED_UNIT_ELEMENT(#2509,-3.);
#1355=DERIVED_UNIT_ELEMENT(#1359,1.);
#1356=DERIVED_UNIT_ELEMENT(#2509,-3.);
#1357=DERIVED_UNIT_ELEMENT(#1359,1.);
#1358=DERIVED_UNIT_ELEMENT(#2509,-3.);
#1359=(
MASS_UNIT()
NAMED_UNIT(*)
SI_UNIT(.KILO.,.GRAM.)
);
#1360=DERIVED_UNIT((#1339,#1340));
#1361=DERIVED_UNIT((#1341,#1342));
#1362=DERIVED_UNIT((#1343,#1344));
#1363=DERIVED_UNIT((#1345,#1346));
#1364=DERIVED_UNIT((#1347,#1348));
#1365=DERIVED_UNIT((#1349,#1350));
#1366=DERIVED_UNIT((#1351,#1352));
#1367=DERIVED_UNIT((#1353,#1354));
#1368=DERIVED_UNIT((#1355,#1356));
#1369=DERIVED_UNIT((#1357,#1358));
#1370=MEASURE_REPRESENTATION_ITEM('density measure',
POSITIVE_RATIO_MEASURE(7850.),#1360);
#1371=MEASURE_REPRESENTATION_ITEM('density measure',
POSITIVE_RATIO_MEASURE(7850.),#1361);
#1372=MEASURE_REPRESENTATION_ITEM('density measure',
POSITIVE_RATIO_MEASURE(7850.),#1362);
#1373=MEASURE_REPRESENTATION_ITEM('density measure',
POSITIVE_RATIO_MEASURE(7850.),#1363);
#1374=MEASURE_REPRESENTATION_ITEM('density measure',
POSITIVE_RATIO_MEASURE(7850.),#1364);
#1375=MEASURE_REPRESENTATION_ITEM('density measure',
POSITIVE_RATIO_MEASURE(7850.),#1365);
#1376=MEASURE_REPRESENTATION_ITEM('density measure',
POSITIVE_RATIO_MEASURE(7850.),#1366);
#1377=MEASURE_REPRESENTATION_ITEM('density measure',
POSITIVE_RATIO_MEASURE(7850.),#1367);
#1378=MEASURE_REPRESENTATION_ITEM('density measure',
POSITIVE_RATIO_MEASURE(7850.),#1368);
#1379=MEASURE_REPRESENTATION_ITEM('density measure',
POSITIVE_RATIO_MEASURE(7850.),#1369);
#1380=PROPERTY_DEFINITION_REPRESENTATION(#1430,#1400);
#1381=PROPERTY_DEFINITION_REPRESENTATION(#1431,#1401);
#1382=PROPERTY_DEFINITION_REPRESENTATION(#1432,#1402);
#1383=PROPERTY_DEFINITION_REPRESENTATION(#1433,#1403);
#1384=PROPERTY_DEFINITION_REPRESENTATION(#1434,#1404);
#1385=PROPERTY_DEFINITION_REPRESENTATION(#1435,#1405);
#1386=PROPERTY_DEFINITION_REPRESENTATION(#1436,#1406);
#1387=PROPERTY_DEFINITION_REPRESENTATION(#1437,#1407);
#1388=PROPERTY_DEFINITION_REPRESENTATION(#1438,#1408);
#1389=PROPERTY_DEFINITION_REPRESENTATION(#1439,#1409);
#1390=PROPERTY_DEFINITION_REPRESENTATION(#1440,#1410);
#1391=PROPERTY_DEFINITION_REPRESENTATION(#1441,#1411);
#1392=PROPERTY_DEFINITION_REPRESENTATION(#1442,#1412);
#1393=PROPERTY_DEFINITION_REPRESENTATION(#1443,#1413);
#1394=PROPERTY_DEFINITION_REPRESENTATION(#1444,#1414);
#1395=PROPERTY_DEFINITION_REPRESENTATION(#1445,#1415);
#1396=PROPERTY_DEFINITION_REPRESENTATION(#1446,#1416);
#1397=PROPERTY_DEFINITION_REPRESENTATION(#1447,#1417);
#1398=PROPERTY_DEFINITION_REPRESENTATION(#1448,#1418);
#1399=PROPERTY_DEFINITION_REPRESENTATION(#1449,#1419);
#1400=REPRESENTATION('material name',(#1420),#2497);
#1401=REPRESENTATION('density',(#1370),#2497);
#1402=REPRESENTATION('material name',(#1421),#2498);
#1403=REPRESENTATION('density',(#1371),#2498);
#1404=REPRESENTATION('material name',(#1422),#2499);
#1405=REPRESENTATION('density',(#1372),#2499);
#1406=REPRESENTATION('material name',(#1423),#2500);
#1407=REPRESENTATION('density',(#1373),#2500);
#1408=REPRESENTATION('material name',(#1424),#2501);
#1409=REPRESENTATION('density',(#1374),#2501);
#1410=REPRESENTATION('material name',(#1425),#2502);
#1411=REPRESENTATION('density',(#1375),#2502);
#1412=REPRESENTATION('material name',(#1426),#2503);
#1413=REPRESENTATION('density',(#1376),#2503);
#1414=REPRESENTATION('material name',(#1427),#2504);
#1415=REPRESENTATION('density',(#1377),#2504);
#1416=REPRESENTATION('material name',(#1428),#2505);
#1417=REPRESENTATION('density',(#1378),#2505);
#1418=REPRESENTATION('material name',(#1429),#2506);
#1419=REPRESENTATION('density',(#1379),#2506);
#1420=DESCRIPTIVE_REPRESENTATION_ITEM('Steel','Steel');
#1421=DESCRIPTIVE_REPRESENTATION_ITEM('Steel','Steel');
#1422=DESCRIPTIVE_REPRESENTATION_ITEM('Steel','Steel');
#1423=DESCRIPTIVE_REPRESENTATION_ITEM('Steel','Steel');
#1424=DESCRIPTIVE_REPRESENTATION_ITEM('Steel','Steel');
#1425=DESCRIPTIVE_REPRESENTATION_ITEM('Steel','Steel');
#1426=DESCRIPTIVE_REPRESENTATION_ITEM('Steel','Steel');
#1427=DESCRIPTIVE_REPRESENTATION_ITEM('Steel','Steel');
#1428=DESCRIPTIVE_REPRESENTATION_ITEM('Steel','Steel');
#1429=DESCRIPTIVE_REPRESENTATION_ITEM('Steel','Steel');
#1430=PROPERTY_DEFINITION('material property','material name',#2586);
#1431=PROPERTY_DEFINITION('material property','density of part',#2586);
#1432=PROPERTY_DEFINITION('material property','material name',#2587);
#1433=PROPERTY_DEFINITION('material property','density of part',#2587);
#1434=PROPERTY_DEFINITION('material property','material name',#2588);
#1435=PROPERTY_DEFINITION('material property','density of part',#2588);
#1436=PROPERTY_DEFINITION('material property','material name',#2589);
#1437=PROPERTY_DEFINITION('material property','density of part',#2589);
#1438=PROPERTY_DEFINITION('material property','material name',#2590);
#1439=PROPERTY_DEFINITION('material property','density of part',#2590);
#1440=PROPERTY_DEFINITION('material property','material name',#2591);
#1441=PROPERTY_DEFINITION('material property','density of part',#2591);
#1442=PROPERTY_DEFINITION('material property','material name',#2592);
#1443=PROPERTY_DEFINITION('material property','density of part',#2592);
#1444=PROPERTY_DEFINITION('material property','material name',#2593);
#1445=PROPERTY_DEFINITION('material property','density of part',#2593);
#1446=PROPERTY_DEFINITION('material property','material name',#2594);
#1447=PROPERTY_DEFINITION('material property','density of part',#2594);
#1448=PROPERTY_DEFINITION('material property','material name',#2595);
#1449=PROPERTY_DEFINITION('material property','density of part',#2595);
#1450=AXIS2_PLACEMENT_3D('',#2085,#1643,#1644);
#1451=AXIS2_PLACEMENT_3D('',#2086,#1645,#1646);
#1452=AXIS2_PLACEMENT_3D('',#2087,#1647,#1648);
#1453=AXIS2_PLACEMENT_3D('',#2089,#1649,#1650);
#1454=AXIS2_PLACEMENT_3D('',#2092,#1652,#1653);
#1455=AXIS2_PLACEMENT_3D('',#2093,#1654,#1655);
#1456=AXIS2_PLACEMENT_3D('',#2095,#1656,#1657);
#1457=AXIS2_PLACEMENT_3D('',#2098,#1659,#1660);
#1458=AXIS2_PLACEMENT_3D('',#2099,#1661,#1662);
#1459=AXIS2_PLACEMENT_3D('',#2100,#1663,#1664);
#1460=AXIS2_PLACEMENT_3D('',#2101,#1665,#1666);
#1461=AXIS2_PLACEMENT_3D('',#2102,#1667,#1668);
#1462=AXIS2_PLACEMENT_3D('',#2104,#1669,#1670);
#1463=AXIS2_PLACEMENT_3D('',#2107,#1672,#1673);
#1464=AXIS2_PLACEMENT_3D('',#2108,#1674,#1675);
#1465=AXIS2_PLACEMENT_3D('',#2110,#1676,#1677);
#1466=AXIS2_PLACEMENT_3D('',#2113,#1679,#1680);
#1467=AXIS2_PLACEMENT_3D('',#2114,#1681,#1682);
#1468=AXIS2_PLACEMENT_3D('',#2116,#1683,#1684);
#1469=AXIS2_PLACEMENT_3D('',#2119,#1686,#1687);
#1470=AXIS2_PLACEMENT_3D('',#2120,#1688,#1689);
#1471=AXIS2_PLACEMENT_3D('',#2122,#1690,#1691);
#1472=AXIS2_PLACEMENT_3D('',#2125,#1693,#1694);
#1473=AXIS2_PLACEMENT_3D('',#2126,#1695,#1696);
#1474=AXIS2_PLACEMENT_3D('',#2128,#1697,#1698);
#1475=AXIS2_PLACEMENT_3D('',#2131,#1700,#1701);
#1476=AXIS2_PLACEMENT_3D('',#2132,#1702,#1703);
#1477=AXIS2_PLACEMENT_3D('',#2134,#1704,#1705);
#1478=AXIS2_PLACEMENT_3D('',#2137,#1707,#1708);
#1479=AXIS2_PLACEMENT_3D('',#2138,#1709,#1710);
#1480=AXIS2_PLACEMENT_3D('',#2139,#1711,#1712);
#1481=AXIS2_PLACEMENT_3D('',#2140,#1713,#1714);
#1482=AXIS2_PLACEMENT_3D('',#2141,#1715,#1716);
#1483=AXIS2_PLACEMENT_3D('',#2143,#1717,#1718);
#1484=AXIS2_PLACEMENT_3D('',#2146,#1720,#1721);
#1485=AXIS2_PLACEMENT_3D('',#2147,#1722,#1723);
#1486=AXIS2_PLACEMENT_3D('',#2149,#1724,#1725);
#1487=AXIS2_PLACEMENT_3D('',#2152,#1727,#1728);
#1488=AXIS2_PLACEMENT_3D('',#2153,#1729,#1730);
#1489=AXIS2_PLACEMENT_3D('',#2155,#1731,#1732);
#1490=AXIS2_PLACEMENT_3D('',#2158,#1734,#1735);
#1491=AXIS2_PLACEMENT_3D('',#2159,#1736,#1737);
#1492=AXIS2_PLACEMENT_3D('',#2161,#1738,#1739);
#1493=AXIS2_PLACEMENT_3D('',#2164,#1741,#1742);
#1494=AXIS2_PLACEMENT_3D('',#2165,#1743,#1744);
#1495=AXIS2_PLACEMENT_3D('',#2167,#1745,#1746);
#1496=AXIS2_PLACEMENT_3D('',#2170,#1748,#1749);
#1497=AXIS2_PLACEMENT_3D('',#2171,#1750,#1751);
#1498=AXIS2_PLACEMENT_3D('',#2173,#1752,#1753);
#1499=AXIS2_PLACEMENT_3D('',#2176,#1755,#1756);
#1500=AXIS2_PLACEMENT_3D('',#2177,#1757,#1758);
#1501=AXIS2_PLACEMENT_3D('',#2178,#1759,#1760);
#1502=AXIS2_PLACEMENT_3D('',#2179,#1761,#1762);
#1503=AXIS2_PLACEMENT_3D('',#2180,#1763,#1764);
#1504=AXIS2_PLACEMENT_3D('',#2182,#1765,#1766);
#1505=AXIS2_PLACEMENT_3D('',#2185,#1768,#1769);
#1506=AXIS2_PLACEMENT_3D('',#2186,#1770,#1771);
#1507=AXIS2_PLACEMENT_3D('',#2188,#1772,#1773);
#1508=AXIS2_PLACEMENT_3D('',#2191,#1775,#1776);
#1509=AXIS2_PLACEMENT_3D('',#2192,#1777,#1778);
#1510=AXIS2_PLACEMENT_3D('',#2194,#1779,#1780);
#1511=AXIS2_PLACEMENT_3D('',#2197,#1782,#1783);
#1512=AXIS2_PLACEMENT_3D('',#2198,#1784,#1785);
#1513=AXIS2_PLACEMENT_3D('',#2200,#1786,#1787);
#1514=AXIS2_PLACEMENT_3D('',#2203,#1789,#1790);
#1515=AXIS2_PLACEMENT_3D('',#2204,#1791,#1792);
#1516=AXIS2_PLACEMENT_3D('',#2206,#1793,#1794);
#1517=AXIS2_PLACEMENT_3D('',#2209,#1796,#1797);
#1518=AXIS2_PLACEMENT_3D('',#2210,#1798,#1799);
#1519=AXIS2_PLACEMENT_3D('',#2212,#1800,#1801);
#1520=AXIS2_PLACEMENT_3D('',#2215,#1803,#1804);
#1521=AXIS2_PLACEMENT_3D('',#2216,#1805,#1806);
#1522=AXIS2_PLACEMENT_3D('',#2217,#1807,#1808);
#1523=AXIS2_PLACEMENT_3D('',#2218,#1809,#1810);
#1524=AXIS2_PLACEMENT_3D('',#2219,#1811,#1812);
#1525=AXIS2_PLACEMENT_3D('',#2221,#1813,#1814);
#1526=AXIS2_PLACEMENT_3D('',#2224,#1816,#1817);
#1527=AXIS2_PLACEMENT_3D('',#2225,#1818,#1819);
#1528=AXIS2_PLACEMENT_3D('',#2227,#1820,#1821);
#1529=AXIS2_PLACEMENT_3D('',#2230,#1823,#1824);
#1530=AXIS2_PLACEMENT_3D('',#2231,#1825,#1826);
#1531=AXIS2_PLACEMENT_3D('',#2233,#1827,#1828);
#1532=AXIS2_PLACEMENT_3D('',#2236,#1830,#1831);
#1533=AXIS2_PLACEMENT_3D('',#2237,#1832,#1833);
#1534=AXIS2_PLACEMENT_3D('',#2239,#1834,#1835);
#1535=AXIS2_PLACEMENT_3D('',#2242,#1837,#1838);
#1536=AXIS2_PLACEMENT_3D('',#2243,#1839,#1840);
#1537=AXIS2_PLACEMENT_3D('',#2245,#1841,#1842);
#1538=AXIS2_PLACEMENT_3D('',#2248,#1844,#1845);
#1539=AXIS2_PLACEMENT_3D('',#2249,#1846,#1847);
#1540=AXIS2_PLACEMENT_3D('',#2251,#1848,#1849);
#1541=AXIS2_PLACEMENT_3D('',#2254,#1851,#1852);
#1542=AXIS2_PLACEMENT_3D('',#2255,#1853,#1854);
#1543=AXIS2_PLACEMENT_3D('',#2256,#1855,#1856);
#1544=AXIS2_PLACEMENT_3D('',#2257,#1857,#1858);
#1545=AXIS2_PLACEMENT_3D('',#2258,#1859,#1860);
#1546=AXIS2_PLACEMENT_3D('',#2260,#1861,#1862);
#1547=AXIS2_PLACEMENT_3D('',#2263,#1864,#1865);
#1548=AXIS2_PLACEMENT_3D('',#2264,#1866,#1867);
#1549=AXIS2_PLACEMENT_3D('',#2266,#1868,#1869);
#1550=AXIS2_PLACEMENT_3D('',#2269,#1871,#1872);
#1551=AXIS2_PLACEMENT_3D('',#2270,#1873,#1874);
#1552=AXIS2_PLACEMENT_3D('',#2271,#1875,#1876);
#1553=AXIS2_PLACEMENT_3D('',#2272,#1877,#1878);
#1554=AXIS2_PLACEMENT_3D('',#2273,#1879,#1880);
#1555=AXIS2_PLACEMENT_3D('',#2275,#1881,#1882);
#1556=AXIS2_PLACEMENT_3D('',#2278,#1884,#1885);
#1557=AXIS2_PLACEMENT_3D('',#2279,#1886,#1887);
#1558=AXIS2_PLACEMENT_3D('',#2281,#1888,#1889);
#1559=AXIS2_PLACEMENT_3D('',#2284,#1891,#1892);
#1560=AXIS2_PLACEMENT_3D('',#2285,#1893,#1894);
#1561=AXIS2_PLACEMENT_3D('',#2286,#1895,#1896);
#1562=AXIS2_PLACEMENT_3D('',#2287,#1897,#1898);
#1563=AXIS2_PLACEMENT_3D('',#2288,#1899,#1900);
#1564=AXIS2_PLACEMENT_3D('',#2290,#1901,#1902);
#1565=AXIS2_PLACEMENT_3D('',#2293,#1904,#1905);
#1566=AXIS2_PLACEMENT_3D('',#2294,#1906,#1907);
#1567=AXIS2_PLACEMENT_3D('',#2296,#1908,#1909);
#1568=AXIS2_PLACEMENT_3D('',#2298,#1911,#1912);
#1569=AXIS2_PLACEMENT_3D('',#2299,#1913,#1914);
#1570=AXIS2_PLACEMENT_3D('',#2301,#1915,#1916);
#1571=AXIS2_PLACEMENT_3D('',#2327,#1918,#1919);
#1572=AXIS2_PLACEMENT_3D('',#2333,#1923,#1924);
#1573=AXIS2_PLACEMENT_3D('',#2337,#1927,#1928);
#1574=AXIS2_PLACEMENT_3D('',#2341,#1931,#1932);
#1575=AXIS2_PLACEMENT_3D('',#2345,#1935,#1936);
#1576=AXIS2_PLACEMENT_3D('',#2349,#1939,#1940);
#1577=AXIS2_PLACEMENT_3D('',#2351,#1942,#1943);
#1578=AXIS2_PLACEMENT_3D('',#2352,#1944,#1945);
#1579=AXIS2_PLACEMENT_3D('',#2353,#1946,#1947);
#1580=AXIS2_PLACEMENT_3D('',#2354,#1948,#1949);
#1581=AXIS2_PLACEMENT_3D('',#2356,#1950,#1951);
#1582=AXIS2_PLACEMENT_3D('',#2359,#1953,#1954);
#1583=AXIS2_PLACEMENT_3D('',#2360,#1955,#1956);
#1584=AXIS2_PLACEMENT_3D('',#2362,#1957,#1958);
#1585=AXIS2_PLACEMENT_3D('',#2365,#1960,#1961);
#1586=AXIS2_PLACEMENT_3D('',#2366,#1962,#1963);
#1587=AXIS2_PLACEMENT_3D('',#2367,#1964,#1965);
#1588=AXIS2_PLACEMENT_3D('',#2368,#1966,#1967);
#1589=AXIS2_PLACEMENT_3D('',#2369,#1968,#1969);
#1590=AXIS2_PLACEMENT_3D('',#2381,#1971,#1972);
#1591=AXIS2_PLACEMENT_3D('',#2397,#1973,#1974);
#1592=AXIS2_PLACEMENT_3D('',#2399,#1975,#1976);
#1593=AXIS2_PLACEMENT_3D('',#2425,#1978,#1979);
#1594=AXIS2_PLACEMENT_3D('',#2428,#1982,#1983);
#1595=AXIS2_PLACEMENT_3D('',#2430,#1985,#1986);
#1596=AXIS2_PLACEMENT_3D('',#2432,#1988,#1989);
#1597=AXIS2_PLACEMENT_3D('',#2434,#1990,#1991);
#1598=AXIS2_PLACEMENT_3D('',#2437,#1993,#1994);
#1599=AXIS2_PLACEMENT_3D('',#2438,#1995,#1996);
#1600=AXIS2_PLACEMENT_3D('',#2440,#1998,#1999);
#1601=AXIS2_PLACEMENT_3D('',#2442,#2001,#2002);
#1602=AXIS2_PLACEMENT_3D('',#2443,#2003,#2004);
#1603=AXIS2_PLACEMENT_3D('',#2444,#2005,#2006);
#1604=AXIS2_PLACEMENT_3D('',#2445,#2007,#2008);
#1605=AXIS2_PLACEMENT_3D('',#2446,#2009,#2010);
#1606=AXIS2_PLACEMENT_3D('',#2447,#2011,#2012);
#1607=AXIS2_PLACEMENT_3D('',#2448,#2013,#2014);
#1608=AXIS2_PLACEMENT_3D('',#2449,#2015,#2016);
#1609=AXIS2_PLACEMENT_3D('',#2450,#2017,#2018);
#1610=AXIS2_PLACEMENT_3D('',#2451,#2019,#2020);
#1611=AXIS2_PLACEMENT_3D('',#2452,#2021,#2022);
#1612=AXIS2_PLACEMENT_3D('',#2453,#2023,#2024);
#1613=AXIS2_PLACEMENT_3D('',#2454,#2025,#2026);
#1614=AXIS2_PLACEMENT_3D('',#2455,#2027,#2028);
#1615=AXIS2_PLACEMENT_3D('',#2456,#2029,#2030);
#1616=AXIS2_PLACEMENT_3D('',#2457,#2031,#2032);
#1617=AXIS2_PLACEMENT_3D('',#2458,#2033,#2034);
#1618=AXIS2_PLACEMENT_3D('',#2459,#2035,#2036);
#1619=AXIS2_PLACEMENT_3D('',#2460,#2037,#2038);
#1620=AXIS2_PLACEMENT_3D('',#2461,#2039,#2040);
#1621=AXIS2_PLACEMENT_3D('',#2462,#2041,#2042);
#1622=AXIS2_PLACEMENT_3D('',#2463,#2043,#2044);
#1623=AXIS2_PLACEMENT_3D('',#2464,#2045,#2046);
#1624=AXIS2_PLACEMENT_3D('',#2465,#2047,#2048);
#1625=AXIS2_PLACEMENT_3D('',#2466,#2049,#2050);
#1626=AXIS2_PLACEMENT_3D('',#2467,#2051,#2052);
#1627=AXIS2_PLACEMENT_3D('',#2468,#2053,#2054);
#1628=AXIS2_PLACEMENT_3D('',#2469,#2055,#2056);
#1629=AXIS2_PLACEMENT_3D('',#2470,#2057,#2058);
#1630=AXIS2_PLACEMENT_3D('',#2471,#2059,#2060);
#1631=AXIS2_PLACEMENT_3D('',#2472,#2061,#2062);
#1632=AXIS2_PLACEMENT_3D('',#2473,#2063,#2064);
#1633=AXIS2_PLACEMENT_3D('',#2474,#2065,#2066);
#1634=AXIS2_PLACEMENT_3D('',#2475,#2067,#2068);
#1635=AXIS2_PLACEMENT_3D('',#2476,#2069,#2070);
#1636=AXIS2_PLACEMENT_3D('',#2477,#2071,#2072);
#1637=AXIS2_PLACEMENT_3D('',#2478,#2073,#2074);
#1638=AXIS2_PLACEMENT_3D('',#2479,#2075,#2076);
#1639=AXIS2_PLACEMENT_3D('',#2480,#2077,#2078);
#1640=AXIS2_PLACEMENT_3D('',#2481,#2079,#2080);
#1641=AXIS2_PLACEMENT_3D('',#2482,#2081,#2082);
#1642=AXIS2_PLACEMENT_3D('',#2483,#2083,#2084);
#1643=DIRECTION('axis',(0.,0.,1.));
#1644=DIRECTION('refdir',(1.,0.,0.));
#1645=DIRECTION('axis',(0.,0.,1.));
#1646=DIRECTION('refdir',(1.,0.,0.));
#1647=DIRECTION('center_axis',(1.,0.,0.));
#1648=DIRECTION('ref_axis',(0.,0.,-1.));
#1649=DIRECTION('center_axis',(-1.,0.,0.));
#1650=DIRECTION('ref_axis',(0.,0.,-1.));
#1651=DIRECTION('',(-1.,0.,0.));
#1652=DIRECTION('center_axis',(-1.,0.,0.));
#1653=DIRECTION('ref_axis',(0.,0.,-1.));
#1654=DIRECTION('center_axis',(1.,0.,0.));
#1655=DIRECTION('ref_axis',(0.,0.,-1.));
#1656=DIRECTION('center_axis',(1.,0.,0.));
#1657=DIRECTION('ref_axis',(0.,0.,-1.));
#1658=DIRECTION('',(-1.,0.,0.));
#1659=DIRECTION('center_axis',(1.,0.,0.));
#1660=DIRECTION('ref_axis',(0.,0.,-1.));
#1661=DIRECTION('center_axis',(1.,0.,0.));
#1662=DIRECTION('ref_axis',(0.,0.,-1.));
#1663=DIRECTION('center_axis',(1.,0.,0.));
#1664=DIRECTION('ref_axis',(0.,0.,-1.));
#1665=DIRECTION('axis',(0.,0.,1.));
#1666=DIRECTION('refdir',(1.,0.,0.));
#1667=DIRECTION('center_axis',(1.,0.,0.));
#1668=DIRECTION('ref_axis',(0.,0.,-1.));
#1669=DIRECTION('center_axis',(1.,0.,0.));
#1670=DIRECTION('ref_axis',(0.,0.,-1.));
#1671=DIRECTION('',(1.,0.,0.));
#1672=DIRECTION('center_axis',(-1.,0.,0.));
#1673=DIRECTION('ref_axis',(0.,0.,-1.));
#1674=DIRECTION('center_axis',(1.,0.,0.));
#1675=DIRECTION('ref_axis',(0.,0.,-1.));
#1676=DIRECTION('center_axis',(1.,0.,0.));
#1677=DIRECTION('ref_axis',(0.,0.,-1.));
#1678=DIRECTION('',(1.,0.,0.));
#1679=DIRECTION('center_axis',(-1.,0.,0.));
#1680=DIRECTION('ref_axis',(0.,0.,-1.));
#1681=DIRECTION('center_axis',(1.,0.,0.));
#1682=DIRECTION('ref_axis',(0.,0.,-1.));
#1683=DIRECTION('center_axis',(1.,0.,0.));
#1684=DIRECTION('ref_axis',(0.,0.,-1.));
#1685=DIRECTION('',(1.,0.,0.));
#1686=DIRECTION('center_axis',(-1.,0.,0.));
#1687=DIRECTION('ref_axis',(0.,0.,-1.));
#1688=DIRECTION('center_axis',(1.,0.,0.));
#1689=DIRECTION('ref_axis',(0.,0.,-1.));
#1690=DIRECTION('center_axis',(1.,0.,0.));
#1691=DIRECTION('ref_axis',(0.,0.,-1.));
#1692=DIRECTION('',(1.,0.,0.));
#1693=DIRECTION('center_axis',(-1.,0.,0.));
#1694=DIRECTION('ref_axis',(0.,0.,-1.));
#1695=DIRECTION('center_axis',(1.,0.,0.));
#1696=DIRECTION('ref_axis',(0.,0.,-1.));
#1697=DIRECTION('center_axis',(-1.,0.,0.));
#1698=DIRECTION('ref_axis',(0.,0.,-1.));
#1699=DIRECTION('',(-1.,0.,0.));
#1700=DIRECTION('center_axis',(-1.,0.,0.));
#1701=DIRECTION('ref_axis',(0.,0.,-1.));
#1702=DIRECTION('center_axis',(1.,0.,0.));
#1703=DIRECTION('ref_axis',(0.,0.,-1.));
#1704=DIRECTION('center_axis',(1.,0.,0.));
#1705=DIRECTION('ref_axis',(0.,0.,-1.));
#1706=DIRECTION('',(-1.,0.,0.));
#1707=DIRECTION('center_axis',(1.,0.,0.));
#1708=DIRECTION('ref_axis',(0.,0.,-1.));
#1709=DIRECTION('center_axis',(1.,0.,0.));
#1710=DIRECTION('ref_axis',(0.,0.,-1.));
#1711=DIRECTION('center_axis',(1.,0.,0.));
#1712=DIRECTION('ref_axis',(0.,0.,-1.));
#1713=DIRECTION('axis',(0.,0.,1.));
#1714=DIRECTION('refdir',(1.,0.,0.));
#1715=DIRECTION('center_axis',(1.,0.,0.));
#1716=DIRECTION('ref_axis',(0.,0.,-1.));
#1717=DIRECTION('center_axis',(1.,0.,0.));
#1718=DIRECTION('ref_axis',(0.,0.,-1.));
#1719=DIRECTION('',(1.,0.,0.));
#1720=DIRECTION('center_axis',(-1.,0.,0.));
#1721=DIRECTION('ref_axis',(0.,0.,-1.));
#1722=DIRECTION('center_axis',(1.,0.,0.));
#1723=DIRECTION('ref_axis',(0.,0.,-1.));
#1724=DIRECTION('center_axis',(1.,0.,0.));
#1725=DIRECTION('ref_axis',(0.,0.,-1.));
#1726=DIRECTION('',(1.,0.,0.));
#1727=DIRECTION('center_axis',(-1.,0.,0.));
#1728=DIRECTION('ref_axis',(0.,0.,-1.));
#1729=DIRECTION('center_axis',(1.,0.,0.));
#1730=DIRECTION('ref_axis',(0.,0.,-1.));
#1731=DIRECTION('center_axis',(1.,0.,0.));
#1732=DIRECTION('ref_axis',(0.,0.,-1.));
#1733=DIRECTION('',(1.,0.,0.));
#1734=DIRECTION('center_axis',(-1.,0.,0.));
#1735=DIRECTION('ref_axis',(0.,0.,-1.));
#1736=DIRECTION('center_axis',(1.,0.,0.));
#1737=DIRECTION('ref_axis',(0.,0.,-1.));
#1738=DIRECTION('center_axis',(1.,0.,0.));
#1739=DIRECTION('ref_axis',(0.,0.,-1.));
#1740=DIRECTION('',(1.,0.,0.));
#1741=DIRECTION('center_axis',(-1.,0.,0.));
#1742=DIRECTION('ref_axis',(0.,0.,-1.));
#1743=DIRECTION('center_axis',(1.,0.,0.));
#1744=DIRECTION('ref_axis',(0.,0.,-1.));
#1745=DIRECTION('center_axis',(-1.,0.,0.));
#1746=DIRECTION('ref_axis',(0.,0.,-1.));
#1747=DIRECTION('',(-1.,0.,0.));
#1748=DIRECTION('center_axis',(-1.,0.,0.));
#1749=DIRECTION('ref_axis',(0.,0.,-1.));
#1750=DIRECTION('center_axis',(1.,0.,0.));
#1751=DIRECTION('ref_axis',(0.,0.,-1.));
#1752=DIRECTION('center_axis',(1.,0.,0.));
#1753=DIRECTION('ref_axis',(0.,0.,-1.));
#1754=DIRECTION('',(-1.,0.,0.));
#1755=DIRECTION('center_axis',(1.,0.,0.));
#1756=DIRECTION('ref_axis',(0.,0.,-1.));
#1757=DIRECTION('center_axis',(1.,0.,0.));
#1758=DIRECTION('ref_axis',(0.,0.,-1.));
#1759=DIRECTION('center_axis',(1.,0.,0.));
#1760=DIRECTION('ref_axis',(0.,0.,-1.));
#1761=DIRECTION('axis',(0.,0.,1.));
#1762=DIRECTION('refdir',(1.,0.,0.));
#1763=DIRECTION('center_axis',(1.,0.,0.));
#1764=DIRECTION('ref_axis',(0.,0.,-1.));
#1765=DIRECTION('center_axis',(1.,0.,0.));
#1766=DIRECTION('ref_axis',(0.,0.,-1.));
#1767=DIRECTION('',(1.,0.,0.));
#1768=DIRECTION('center_axis',(-1.,0.,0.));
#1769=DIRECTION('ref_axis',(0.,0.,-1.));
#1770=DIRECTION('center_axis',(1.,0.,0.));
#1771=DIRECTION('ref_axis',(0.,0.,-1.));
#1772=DIRECTION('center_axis',(1.,0.,0.));
#1773=DIRECTION('ref_axis',(0.,0.,-1.));
#1774=DIRECTION('',(1.,0.,0.));
#1775=DIRECTION('center_axis',(-1.,0.,0.));
#1776=DIRECTION('ref_axis',(0.,0.,-1.));
#1777=DIRECTION('center_axis',(1.,0.,0.));
#1778=DIRECTION('ref_axis',(0.,0.,-1.));
#1779=DIRECTION('center_axis',(1.,0.,0.));
#1780=DIRECTION('ref_axis',(0.,0.,-1.));
#1781=DIRECTION('',(1.,0.,0.));
#1782=DIRECTION('center_axis',(-1.,0.,0.));
#1783=DIRECTION('ref_axis',(0.,0.,-1.));
#1784=DIRECTION('center_axis',(1.,0.,0.));
#1785=DIRECTION('ref_axis',(0.,0.,-1.));
#1786=DIRECTION('center_axis',(1.,0.,0.));
#1787=DIRECTION('ref_axis',(0.,0.,-1.));
#1788=DIRECTION('',(1.,0.,0.));
#1789=DIRECTION('center_axis',(-1.,0.,0.));
#1790=DIRECTION('ref_axis',(0.,0.,-1.));
#1791=DIRECTION('center_axis',(1.,0.,0.));
#1792=DIRECTION('ref_axis',(0.,0.,-1.));
#1793=DIRECTION('center_axis',(-1.,0.,0.));
#1794=DIRECTION('ref_axis',(0.,0.,-1.));
#1795=DIRECTION('',(-1.,0.,0.));
#1796=DIRECTION('center_axis',(-1.,0.,0.));
#1797=DIRECTION('ref_axis',(0.,0.,-1.));
#1798=DIRECTION('center_axis',(1.,0.,0.));
#1799=DIRECTION('ref_axis',(0.,0.,-1.));
#1800=DIRECTION('center_axis',(1.,0.,0.));
#1801=DIRECTION('ref_axis',(0.,0.,-1.));
#1802=DIRECTION('',(-1.,0.,0.));
#1803=DIRECTION('center_axis',(1.,0.,0.));
#1804=DIRECTION('ref_axis',(0.,0.,-1.));
#1805=DIRECTION('center_axis',(1.,0.,0.));
#1806=DIRECTION('ref_axis',(0.,0.,-1.));
#1807=DIRECTION('center_axis',(1.,0.,0.));
#1808=DIRECTION('ref_axis',(0.,0.,-1.));
#1809=DIRECTION('axis',(0.,0.,1.));
#1810=DIRECTION('refdir',(1.,0.,0.));
#1811=DIRECTION('center_axis',(1.,0.,0.));
#1812=DIRECTION('ref_axis',(0.,0.,-1.));
#1813=DIRECTION('center_axis',(1.,0.,0.));
#1814=DIRECTION('ref_axis',(0.,0.,-1.));
#1815=DIRECTION('',(1.,0.,0.));
#1816=DIRECTION('center_axis',(-1.,0.,0.));
#1817=DIRECTION('ref_axis',(0.,0.,-1.));
#1818=DIRECTION('center_axis',(1.,0.,0.));
#1819=DIRECTION('ref_axis',(0.,0.,-1.));
#1820=DIRECTION('center_axis',(1.,0.,0.));
#1821=DIRECTION('ref_axis',(0.,0.,-1.));
#1822=DIRECTION('',(1.,0.,0.));
#1823=DIRECTION('center_axis',(-1.,0.,0.));
#1824=DIRECTION('ref_axis',(0.,0.,-1.));
#1825=DIRECTION('center_axis',(1.,0.,0.));
#1826=DIRECTION('ref_axis',(0.,0.,-1.));
#1827=DIRECTION('center_axis',(1.,0.,0.));
#1828=DIRECTION('ref_axis',(0.,0.,-1.));
#1829=DIRECTION('',(1.,0.,0.));
#1830=DIRECTION('center_axis',(-1.,0.,0.));
#1831=DIRECTION('ref_axis',(0.,0.,-1.));
#1832=DIRECTION('center_axis',(1.,0.,0.));
#1833=DIRECTION('ref_axis',(0.,0.,-1.));
#1834=DIRECTION('center_axis',(1.,0.,0.));
#1835=DIRECTION('ref_axis',(0.,0.,-1.));
#1836=DIRECTION('',(1.,0.,0.));
#1837=DIRECTION('center_axis',(-1.,0.,0.));
#1838=DIRECTION('ref_axis',(0.,0.,-1.));
#1839=DIRECTION('center_axis',(1.,0.,0.));
#1840=DIRECTION('ref_axis',(0.,0.,-1.));
#1841=DIRECTION('center_axis',(-1.,0.,0.));
#1842=DIRECTION('ref_axis',(0.,0.,-1.));
#1843=DIRECTION('',(-1.,0.,0.));
#1844=DIRECTION('center_axis',(-1.,0.,0.));
#1845=DIRECTION('ref_axis',(0.,0.,-1.));
#1846=DIRECTION('center_axis',(1.,0.,0.));
#1847=DIRECTION('ref_axis',(0.,0.,-1.));
#1848=DIRECTION('center_axis',(1.,0.,0.));
#1849=DIRECTION('ref_axis',(0.,0.,-1.));
#1850=DIRECTION('',(-1.,0.,0.));
#1851=DIRECTION('center_axis',(1.,0.,0.));
#1852=DIRECTION('ref_axis',(0.,0.,-1.));
#1853=DIRECTION('center_axis',(1.,0.,0.));
#1854=DIRECTION('ref_axis',(0.,0.,-1.));
#1855=DIRECTION('center_axis',(1.,0.,0.));
#1856=DIRECTION('ref_axis',(0.,0.,-1.));
#1857=DIRECTION('axis',(0.,0.,1.));
#1858=DIRECTION('refdir',(1.,0.,0.));
#1859=DIRECTION('center_axis',(1.,0.,0.));
#1860=DIRECTION('ref_axis',(0.,0.,-1.));
#1861=DIRECTION('center_axis',(-1.,0.,0.));
#1862=DIRECTION('ref_axis',(0.,0.,-1.));
#1863=DIRECTION('',(-1.,0.,0.));
#1864=DIRECTION('center_axis',(-1.,0.,0.));
#1865=DIRECTION('ref_axis',(0.,0.,-1.));
#1866=DIRECTION('center_axis',(1.,0.,0.));
#1867=DIRECTION('ref_axis',(0.,0.,-1.));
#1868=DIRECTION('center_axis',(1.,0.,0.));
#1869=DIRECTION('ref_axis',(0.,0.,-1.));
#1870=DIRECTION('',(-1.,0.,0.));
#1871=DIRECTION('center_axis',(1.,0.,0.));
#1872=DIRECTION('ref_axis',(0.,0.,-1.));
#1873=DIRECTION('center_axis',(1.,0.,0.));
#1874=DIRECTION('ref_axis',(0.,0.,-1.));
#1875=DIRECTION('center_axis',(1.,0.,0.));
#1876=DIRECTION('ref_axis',(0.,0.,-1.));
#1877=DIRECTION('axis',(0.,0.,1.));
#1878=DIRECTION('refdir',(1.,0.,0.));
#1879=DIRECTION('center_axis',(1.,0.,0.));
#1880=DIRECTION('ref_axis',(0.,0.,-1.));
#1881=DIRECTION('center_axis',(-1.,0.,0.));
#1882=DIRECTION('ref_axis',(0.,0.,-1.));
#1883=DIRECTION('',(-1.,0.,0.));
#1884=DIRECTION('center_axis',(-1.,0.,0.));
#1885=DIRECTION('ref_axis',(0.,0.,-1.));
#1886=DIRECTION('center_axis',(1.,0.,0.));
#1887=DIRECTION('ref_axis',(0.,0.,-1.));
#1888=DIRECTION('center_axis',(1.,0.,0.));
#1889=DIRECTION('ref_axis',(0.,0.,-1.));
#1890=DIRECTION('',(-1.,0.,0.));
#1891=DIRECTION('center_axis',(1.,0.,0.));
#1892=DIRECTION('ref_axis',(0.,0.,-1.));
#1893=DIRECTION('center_axis',(1.,0.,0.));
#1894=DIRECTION('ref_axis',(0.,0.,-1.));
#1895=DIRECTION('center_axis',(1.,0.,0.));
#1896=DIRECTION('ref_axis',(0.,0.,-1.));
#1897=DIRECTION('axis',(0.,0.,1.));
#1898=DIRECTION('refdir',(1.,0.,0.));
#1899=DIRECTION('center_axis',(0.,-1.,0.));
#1900=DIRECTION('ref_axis',(1.,0.,0.));
#1901=DIRECTION('center_axis',(0.,1.,0.));
#1902=DIRECTION('ref_axis',(1.,0.,0.));
#1903=DIRECTION('',(0.,1.,0.));
#1904=DIRECTION('center_axis',(0.,-1.,0.));
#1905=DIRECTION('ref_axis',(1.,0.,0.));
#1906=DIRECTION('center_axis',(0.,1.,0.));
#1907=DIRECTION('ref_axis',(1.,0.,0.));
#1908=DIRECTION('center_axis',(0.,-1.,0.));
#1909=DIRECTION('ref_axis',(1.,0.,0.));
#1910=DIRECTION('',(-0.707106781186549,0.707106781186546,-8.65956056235496E-17));
#1911=DIRECTION('center_axis',(0.,-1.,0.));
#1912=DIRECTION('ref_axis',(0.,0.,-1.));
#1913=DIRECTION('center_axis',(0.,-1.,0.));
#1914=DIRECTION('ref_axis',(1.,0.,0.));
#1915=DIRECTION('center_axis',(0.,1.,0.));
#1916=DIRECTION('ref_axis',(1.,0.,0.));
#1917=DIRECTION('',(-0.866025403784439,-0.5,-1.06057523872491E-16));
#1918=DIRECTION('center_axis',(1.4792020664489E-16,0.,-1.));
#1919=DIRECTION('ref_axis',(-1.,0.,-1.4792020664489E-16));
#1920=DIRECTION('',(0.,1.,0.));
#1921=DIRECTION('',(-1.,0.,-1.4792020664489E-16));
#1922=DIRECTION('',(0.,1.,0.));
#1923=DIRECTION('center_axis',(0.866025403784439,0.,-0.5));
#1924=DIRECTION('ref_axis',(-0.5,0.,-0.866025403784439));
#1925=DIRECTION('',(0.,1.,0.));
#1926=DIRECTION('',(-0.5,0.,-0.866025403784439));
#1927=DIRECTION('center_axis',(0.866025403784439,0.,0.5));
#1928=DIRECTION('ref_axis',(0.5,0.,-0.866025403784439));
#1929=DIRECTION('',(0.,1.,0.));
#1930=DIRECTION('',(0.5,0.,-0.866025403784439));
#1931=DIRECTION('center_axis',(-2.95840413289779E-16,0.,1.));
#1932=DIRECTION('ref_axis',(1.,0.,2.95840413289779E-16));
#1933=DIRECTION('',(0.,1.,0.));
#1934=DIRECTION('',(1.,0.,2.95840413289779E-16));
#1935=DIRECTION('center_axis',(-0.866025403784439,0.,0.5));
#1936=DIRECTION('ref_axis',(0.5,0.,0.866025403784439));
#1937=DIRECTION('',(0.,1.,0.));
#1938=DIRECTION('',(0.5,0.,0.866025403784439));
#1939=DIRECTION('center_axis',(-0.866025403784439,0.,-0.5));
#1940=DIRECTION('ref_axis',(-0.5,0.,0.866025403784439));
#1941=DIRECTION('',(-0.5,0.,0.866025403784439));
#1942=DIRECTION('center_axis',(0.,1.,0.));
#1943=DIRECTION('ref_axis',(0.,0.,1.));
#1944=DIRECTION('center_axis',(0.,1.,0.));
#1945=DIRECTION('ref_axis',(1.,0.,0.));
#1946=DIRECTION('axis',(0.,0.,1.));
#1947=DIRECTION('refdir',(1.,0.,0.));
#1948=DIRECTION('center_axis',(0.,1.,0.));
#1949=DIRECTION('ref_axis',(1.,0.,0.));
#1950=DIRECTION('center_axis',(0.,-1.,0.));
#1951=DIRECTION('ref_axis',(1.,0.,0.));
#1952=DIRECTION('',(0.,-1.,0.));
#1953=DIRECTION('center_axis',(0.,-1.,0.));
#1954=DIRECTION('ref_axis',(1.,0.,0.));
#1955=DIRECTION('center_axis',(0.,1.,0.));
#1956=DIRECTION('ref_axis',(1.,0.,0.));
#1957=DIRECTION('center_axis',(0.,1.,0.));
#1958=DIRECTION('ref_axis',(1.,0.,0.));
#1959=DIRECTION('',(0.,-1.,0.));
#1960=DIRECTION('center_axis',(0.,1.,0.));
#1961=DIRECTION('ref_axis',(1.,0.,0.));
#1962=DIRECTION('center_axis',(0.,1.,0.));
#1963=DIRECTION('ref_axis',(1.,0.,0.));
#1964=DIRECTION('center_axis',(0.,1.,0.));
#1965=DIRECTION('ref_axis',(1.,0.,0.));
#1966=DIRECTION('axis',(0.,0.,1.));
#1967=DIRECTION('refdir',(1.,0.,0.));
#1968=DIRECTION('center_axis',(0.,1.,0.));
#1969=DIRECTION('ref_axis',(1.,0.,0.));
#1970=DIRECTION('',(0.866025403784439,-0.5,1.06057523872491E-16));
#1971=DIRECTION('center_axis',(0.,-1.,0.));
#1972=DIRECTION('ref_axis',(1.,0.,0.));
#1973=DIRECTION('center_axis',(0.,-1.,0.));
#1974=DIRECTION('ref_axis',(1.,0.,0.));
#1975=DIRECTION('center_axis',(0.,1.,0.));
#1976=DIRECTION('ref_axis',(1.,0.,0.));
#1977=DIRECTION('',(-0.866025403784439,-0.5,-1.06057523872491E-16));
#1978=DIRECTION('center_axis',(1.4792020664489E-16,0.,-1.));
#1979=DIRECTION('ref_axis',(-1.,0.,-1.4792020664489E-16));
#1980=DIRECTION('',(0.,1.,0.));
#1981=DIRECTION('',(0.,1.,0.));
#1982=DIRECTION('center_axis',(-0.866025403784439,0.,-0.5));
#1983=DIRECTION('ref_axis',(-0.5,0.,0.866025403784439));
#1984=DIRECTION('',(0.,1.,0.));
#1985=DIRECTION('center_axis',(-0.866025403784439,0.,0.5));
#1986=DIRECTION('ref_axis',(0.5,0.,0.866025403784439));
#1987=DIRECTION('',(0.,1.,0.));
#1988=DIRECTION('center_axis',(0.,1.,0.));
#1989=DIRECTION('ref_axis',(1.,0.,0.));
#1990=DIRECTION('center_axis',(0.,1.,0.));
#1991=DIRECTION('ref_axis',(1.,0.,0.));
#1992=DIRECTION('',(0.,-1.,0.));
#1993=DIRECTION('center_axis',(0.,1.,0.));
#1994=DIRECTION('ref_axis',(1.,0.,0.));
#1995=DIRECTION('center_axis',(-2.95840413289779E-16,0.,1.));
#1996=DIRECTION('ref_axis',(1.,0.,2.95840413289779E-16));
#1997=DIRECTION('',(0.,1.,0.));
#1998=DIRECTION('center_axis',(0.866025403784439,0.,-0.5));
#1999=DIRECTION('ref_axis',(-0.5,0.,-0.866025403784439));
#2000=DIRECTION('',(0.,1.,0.));
#2001=DIRECTION('center_axis',(0.866025403784439,0.,0.5));
#2002=DIRECTION('ref_axis',(0.5,0.,-0.866025403784439));
#2003=DIRECTION('center_axis',(0.,1.,0.));
#2004=DIRECTION('ref_axis',(1.,0.,0.));
#2005=DIRECTION('center_axis',(0.,1.,0.));
#2006=DIRECTION('ref_axis',(1.,0.,0.));
#2007=DIRECTION('',(0.,0.,1.));
#2008=DIRECTION('',(1.,0.,0.));
#2009=DIRECTION('',(0.,0.,1.));
#2010=DIRECTION('',(1.,0.,0.));
#2011=DIRECTION('',(0.,0.,1.));
#2012=DIRECTION('',(1.,0.,0.));
#2013=DIRECTION('',(0.,0.,1.));
#2014=DIRECTION('',(1.,0.,0.));
#2015=DIRECTION('',(0.,0.,1.));
#2016=DIRECTION('',(1.,0.,0.));
#2017=DIRECTION('',(0.,0.,1.));
#2018=DIRECTION('',(1.,0.,0.));
#2019=DIRECTION('',(0.,0.,1.));
#2020=DIRECTION('',(1.,0.,0.));
#2021=DIRECTION('',(0.,0.,1.));
#2022=DIRECTION('',(2.22044604925031E-16,-1.,0.));
#2023=DIRECTION('',(0.,0.,1.));
#2024=DIRECTION('',(2.22044604925031E-16,1.,0.));
#2025=DIRECTION('',(0.,0.,1.));
#2026=DIRECTION('',(2.22044604925031E-16,-1.,0.));
#2027=DIRECTION('',(0.,0.,1.));
#2028=DIRECTION('',(2.22044604925031E-16,-1.,0.));
#2029=DIRECTION('',(0.,0.,1.));
#2030=DIRECTION('',(2.22044604925031E-16,-1.,0.));
#2031=DIRECTION('',(0.,0.,1.));
#2032=DIRECTION('',(2.22044604925031E-16,1.,0.));
#2033=DIRECTION('',(0.,0.,1.));
#2034=DIRECTION('',(2.22044604925031E-16,-1.,0.));
#2035=DIRECTION('',(0.,0.,1.));
#2036=DIRECTION('',(2.22044604925031E-16,-1.,0.));
#2037=DIRECTION('',(0.,0.,1.));
#2038=DIRECTION('',(2.22044604925031E-16,-1.,0.));
#2039=DIRECTION('',(0.,0.,1.));
#2040=DIRECTION('',(2.22044604925031E-16,1.,0.));
#2041=DIRECTION('',(0.,0.,1.));
#2042=DIRECTION('',(2.22044604925031E-16,-1.,0.));
#2043=DIRECTION('',(0.,0.,1.));
#2044=DIRECTION('',(2.22044604925031E-16,-1.,0.));
#2045=DIRECTION('',(0.,0.,1.));
#2046=DIRECTION('',(2.22044604925031E-16,-1.,0.));
#2047=DIRECTION('',(0.,0.,1.));
#2048=DIRECTION('',(2.22044604925031E-16,1.,0.));
#2049=DIRECTION('',(0.,0.,1.));
#2050=DIRECTION('',(2.22044604925031E-16,-1.,0.));
#2051=DIRECTION('',(0.,0.,1.));
#2052=DIRECTION('',(2.22044604925031E-16,-1.,0.));
#2053=DIRECTION('',(0.,0.,1.));
#2054=DIRECTION('',(2.22044604925031E-16,-1.,0.));
#2055=DIRECTION('',(0.,0.,1.));
#2056=DIRECTION('',(2.22044604925031E-16,1.,0.));
#2057=DIRECTION('',(0.,0.,1.));
#2058=DIRECTION('',(2.22044604925031E-16,-1.,0.));
#2059=DIRECTION('',(0.,0.,1.));
#2060=DIRECTION('',(2.22044604925031E-16,-1.,0.));
#2061=DIRECTION('',(0.,0.,1.));
#2062=DIRECTION('',(2.22044604925031E-16,-1.,0.));
#2063=DIRECTION('',(0.,0.,1.));
#2064=DIRECTION('',(2.22044604925031E-16,1.,0.));
#2065=DIRECTION('',(0.,0.,1.));
#2066=DIRECTION('',(2.22044604925031E-16,-1.,0.));
#2067=DIRECTION('',(0.,0.,1.));
#2068=DIRECTION('',(2.22044604925031E-16,-1.,0.));
#2069=DIRECTION('',(0.,0.,1.));
#2070=DIRECTION('',(2.22044604925031E-16,-1.,0.));
#2071=DIRECTION('',(0.,0.,1.));
#2072=DIRECTION('',(2.22044604925031E-16,1.,0.));
#2073=DIRECTION('',(0.,0.,1.));
#2074=DIRECTION('',(2.22044604925031E-16,-1.,0.));
#2075=DIRECTION('',(0.,0.,1.));
#2076=DIRECTION('',(2.22044604925031E-16,-1.,0.));
#2077=DIRECTION('',(0.,0.,1.));
#2078=DIRECTION('',(2.22044604925031E-16,-1.,0.));
#2079=DIRECTION('',(0.,0.,1.));
#2080=DIRECTION('',(2.22044604925031E-16,1.,0.));
#2081=DIRECTION('',(0.,0.,1.));
#2082=DIRECTION('',(2.22044604925031E-16,-1.,0.));
#2083=DIRECTION('',(0.,0.,1.));
#2084=DIRECTION('',(2.22044604925031E-16,-1.,0.));
#2085=CARTESIAN_POINT('',(0.,0.,0.));
#2086=CARTESIAN_POINT('',(0.,0.,0.));
#2087=CARTESIAN_POINT('Origin',(-10.,0.,0.));
#2088=CARTESIAN_POINT('',(10.,-9.67470971326409E-17,0.79));
#2089=CARTESIAN_POINT('Origin',(10.,0.,0.));
#2090=CARTESIAN_POINT('',(-10.,-9.67470971326409E-17,0.79));
#2091=CARTESIAN_POINT('',(-10.,-9.67470971326409E-17,0.79));
#2092=CARTESIAN_POINT('Origin',(-10.,0.,0.));
#2093=CARTESIAN_POINT('Origin',(-10.,0.,0.));
#2094=CARTESIAN_POINT('',(10.,-1.30424884109193E-16,1.065));
#2095=CARTESIAN_POINT('Origin',(10.,0.,0.));
#2096=CARTESIAN_POINT('',(-10.,-1.30424884109193E-16,1.065));
#2097=CARTESIAN_POINT('',(-10.,-1.30424884109193E-16,1.065));
#2098=CARTESIAN_POINT('Origin',(-10.,0.,0.));
#2099=CARTESIAN_POINT('Origin',(10.,0.,0.));
#2100=CARTESIAN_POINT('Origin',(-10.,0.,0.));
#2101=CARTESIAN_POINT('',(0.,0.,0.));
#2102=CARTESIAN_POINT('Origin',(-10.1,-1.90918830920368,-1.90918830920368));
#2103=CARTESIAN_POINT('',(-10.,-1.90918830920368,-1.46918830920368));
#2104=CARTESIAN_POINT('Origin',(-10.,-1.90918830920368,-1.90918830920368));
#2105=CARTESIAN_POINT('',(-9.2,-1.90918830920368,-1.46918830920368));
#2106=CARTESIAN_POINT('',(-10.1,-1.90918830920368,-1.46918830920368));
#2107=CARTESIAN_POINT('Origin',(-9.2,-1.90918830920368,-1.90918830920368));
#2108=CARTESIAN_POINT('Origin',(-10.1,-1.90918830920368,1.90918830920368));
#2109=CARTESIAN_POINT('',(-10.,-1.90918830920368,2.34918830920368));
#2110=CARTESIAN_POINT('Origin',(-10.,-1.90918830920368,1.90918830920368));
#2111=CARTESIAN_POINT('',(-9.2,-1.90918830920368,2.34918830920368));
#2112=CARTESIAN_POINT('',(-10.1,-1.90918830920368,2.34918830920368));
#2113=CARTESIAN_POINT('Origin',(-9.2,-1.90918830920368,1.90918830920368));
#2114=CARTESIAN_POINT('Origin',(-10.1,1.90918830920368,1.90918830920368));
#2115=CARTESIAN_POINT('',(-10.,1.90918830920368,2.34918830920368));
#2116=CARTESIAN_POINT('Origin',(-10.,1.90918830920368,1.90918830920368));
#2117=CARTESIAN_POINT('',(-9.2,1.90918830920368,2.34918830920368));
#2118=CARTESIAN_POINT('',(-10.1,1.90918830920368,2.34918830920368));
#2119=CARTESIAN_POINT('Origin',(-9.2,1.90918830920368,1.90918830920368));
#2120=CARTESIAN_POINT('Origin',(-10.1,1.90918830920368,-1.90918830920368));
#2121=CARTESIAN_POINT('',(-10.,1.90918830920368,-1.46918830920368));
#2122=CARTESIAN_POINT('Origin',(-10.,1.90918830920368,-1.90918830920368));
#2123=CARTESIAN_POINT('',(-9.2,1.90918830920368,-1.46918830920368));
#2124=CARTESIAN_POINT('',(-10.1,1.90918830920368,-1.46918830920368));
#2125=CARTESIAN_POINT('Origin',(-9.2,1.90918830920368,-1.90918830920368));
#2126=CARTESIAN_POINT('Origin',(-10.,0.,0.));
#2127=CARTESIAN_POINT('',(-9.2,-1.30424884109193E-16,1.065));
#2128=CARTESIAN_POINT('Origin',(-9.2,0.,0.));
#2129=CARTESIAN_POINT('',(-10.,-1.30424884109193E-16,1.065));
#2130=CARTESIAN_POINT('',(-10.,-1.30424884109193E-16,1.065));
#2131=CARTESIAN_POINT('Origin',(-10.,0.,0.));
#2132=CARTESIAN_POINT('Origin',(-10.,0.,0.));
#2133=CARTESIAN_POINT('',(-9.2,-4.28626379701574E-16,3.5));
#2134=CARTESIAN_POINT('Origin',(-9.2,0.,0.));
#2135=CARTESIAN_POINT('',(-10.,-4.28626379701574E-16,3.5));
#2136=CARTESIAN_POINT('',(-10.,-4.28626379701574E-16,3.5));
#2137=CARTESIAN_POINT('Origin',(-10.,0.,0.));
#2138=CARTESIAN_POINT('Origin',(-9.2,0.,0.));
#2139=CARTESIAN_POINT('Origin',(-10.,0.,0.));
#2140=CARTESIAN_POINT('',(0.,0.,0.));
#2141=CARTESIAN_POINT('Origin',(9.1,-1.90918830920368,-1.90918830920368));
#2142=CARTESIAN_POINT('',(9.2,-1.90918830920368,-1.46918830920368));
#2143=CARTESIAN_POINT('Origin',(9.2,-1.90918830920368,-1.90918830920368));
#2144=CARTESIAN_POINT('',(10.,-1.90918830920368,-1.46918830920368));
#2145=CARTESIAN_POINT('',(9.1,-1.90918830920368,-1.46918830920368));
#2146=CARTESIAN_POINT('Origin',(10.,-1.90918830920368,-1.90918830920368));
#2147=CARTESIAN_POINT('Origin',(9.1,-1.90918830920368,1.90918830920368));
#2148=CARTESIAN_POINT('',(9.2,-1.90918830920368,2.34918830920368));
#2149=CARTESIAN_POINT('Origin',(9.2,-1.90918830920368,1.90918830920368));
#2150=CARTESIAN_POINT('',(10.,-1.90918830920368,2.34918830920368));
#2151=CARTESIAN_POINT('',(9.1,-1.90918830920368,2.34918830920368));
#2152=CARTESIAN_POINT('Origin',(10.,-1.90918830920368,1.90918830920368));
#2153=CARTESIAN_POINT('Origin',(9.1,1.90918830920368,1.90918830920368));
#2154=CARTESIAN_POINT('',(9.2,1.90918830920368,2.34918830920368));
#2155=CARTESIAN_POINT('Origin',(9.2,1.90918830920368,1.90918830920368));
#2156=CARTESIAN_POINT('',(10.,1.90918830920368,2.34918830920368));
#2157=CARTESIAN_POINT('',(9.1,1.90918830920368,2.34918830920368));
#2158=CARTESIAN_POINT('Origin',(10.,1.90918830920368,1.90918830920368));
#2159=CARTESIAN_POINT('Origin',(9.1,1.90918830920368,-1.90918830920368));
#2160=CARTESIAN_POINT('',(9.2,1.90918830920368,-1.46918830920368));
#2161=CARTESIAN_POINT('Origin',(9.2,1.90918830920368,-1.90918830920368));
#2162=CARTESIAN_POINT('',(10.,1.90918830920368,-1.46918830920368));
#2163=CARTESIAN_POINT('',(9.1,1.90918830920368,-1.46918830920368));
#2164=CARTESIAN_POINT('Origin',(10.,1.90918830920368,-1.90918830920368));
#2165=CARTESIAN_POINT('Origin',(9.2,0.,0.));
#2166=CARTESIAN_POINT('',(10.,-1.30424884109193E-16,1.065));
#2167=CARTESIAN_POINT('Origin',(10.,0.,0.));
#2168=CARTESIAN_POINT('',(9.2,-1.30424884109193E-16,1.065));
#2169=CARTESIAN_POINT('',(9.2,-1.30424884109193E-16,1.065));
#2170=CARTESIAN_POINT('Origin',(9.2,0.,0.));
#2171=CARTESIAN_POINT('Origin',(9.2,0.,0.));
#2172=CARTESIAN_POINT('',(10.,-4.28626379701574E-16,3.5));
#2173=CARTESIAN_POINT('Origin',(10.,0.,0.));
#2174=CARTESIAN_POINT('',(9.2,-4.28626379701574E-16,3.5));
#2175=CARTESIAN_POINT('',(9.2,-4.28626379701574E-16,3.5));
#2176=CARTESIAN_POINT('Origin',(9.2,0.,0.));
#2177=CARTESIAN_POINT('Origin',(10.,0.,0.));
#2178=CARTESIAN_POINT('Origin',(9.2,0.,0.));
#2179=CARTESIAN_POINT('',(0.,0.,0.));
#2180=CARTESIAN_POINT('Origin',(-11.1,-1.90918830920368,-1.90918830920368));
#2181=CARTESIAN_POINT('',(-11.,-1.90918830920368,-1.46918830920368));
#2182=CARTESIAN_POINT('Origin',(-11.,-1.90918830920368,-1.90918830920368));
#2183=CARTESIAN_POINT('',(-10.2,-1.90918830920368,-1.46918830920368));
#2184=CARTESIAN_POINT('',(-11.1,-1.90918830920368,-1.46918830920368));
#2185=CARTESIAN_POINT('Origin',(-10.2,-1.90918830920368,-1.90918830920368));
#2186=CARTESIAN_POINT('Origin',(-11.1,-1.90918830920368,1.90918830920368));
#2187=CARTESIAN_POINT('',(-11.,-1.90918830920368,2.34918830920368));
#2188=CARTESIAN_POINT('Origin',(-11.,-1.90918830920368,1.90918830920368));
#2189=CARTESIAN_POINT('',(-10.2,-1.90918830920368,2.34918830920368));
#2190=CARTESIAN_POINT('',(-11.1,-1.90918830920368,2.34918830920368));
#2191=CARTESIAN_POINT('Origin',(-10.2,-1.90918830920368,1.90918830920368));
#2192=CARTESIAN_POINT('Origin',(-11.1,1.90918830920368,1.90918830920368));
#2193=CARTESIAN_POINT('',(-11.,1.90918830920368,2.34918830920368));
#2194=CARTESIAN_POINT('Origin',(-11.,1.90918830920368,1.90918830920368));
#2195=CARTESIAN_POINT('',(-10.2,1.90918830920368,2.34918830920368));
#2196=CARTESIAN_POINT('',(-11.1,1.90918830920368,2.34918830920368));
#2197=CARTESIAN_POINT('Origin',(-10.2,1.90918830920368,1.90918830920368));
#2198=CARTESIAN_POINT('Origin',(-11.1,1.90918830920368,-1.90918830920368));
#2199=CARTESIAN_POINT('',(-11.,1.90918830920368,-1.46918830920368));
#2200=CARTESIAN_POINT('Origin',(-11.,1.90918830920368,-1.90918830920368));
#2201=CARTESIAN_POINT('',(-10.2,1.90918830920368,-1.46918830920368));
#2202=CARTESIAN_POINT('',(-11.1,1.90918830920368,-1.46918830920368));
#2203=CARTESIAN_POINT('Origin',(-10.2,1.90918830920368,-1.90918830920368));
#2204=CARTESIAN_POINT('Origin',(-11.,0.,0.));
#2205=CARTESIAN_POINT('',(-10.2,-1.30424884109193E-16,1.065));
#2206=CARTESIAN_POINT('Origin',(-10.2,0.,0.));
#2207=CARTESIAN_POINT('',(-11.,-1.30424884109193E-16,1.065));
#2208=CARTESIAN_POINT('',(-11.,-1.30424884109193E-16,1.065));
#2209=CARTESIAN_POINT('Origin',(-11.,0.,0.));
#2210=CARTESIAN_POINT('Origin',(-11.,0.,0.));
#2211=CARTESIAN_POINT('',(-10.2,-4.28626379701574E-16,3.5));
#2212=CARTESIAN_POINT('Origin',(-10.2,0.,0.));
#2213=CARTESIAN_POINT('',(-11.,-4.28626379701574E-16,3.5));
#2214=CARTESIAN_POINT('',(-11.,-4.28626379701574E-16,3.5));
#2215=CARTESIAN_POINT('Origin',(-11.,0.,0.));
#2216=CARTESIAN_POINT('Origin',(-10.2,0.,0.));
#2217=CARTESIAN_POINT('Origin',(-11.,0.,0.));
#2218=CARTESIAN_POINT('',(0.,0.,0.));
#2219=CARTESIAN_POINT('Origin',(10.1,-1.90918830920368,-1.90918830920368));
#2220=CARTESIAN_POINT('',(10.2,-1.90918830920368,-1.46918830920368));
#2221=CARTESIAN_POINT('Origin',(10.2,-1.90918830920368,-1.90918830920368));
#2222=CARTESIAN_POINT('',(11.,-1.90918830920368,-1.46918830920368));
#2223=CARTESIAN_POINT('',(10.1,-1.90918830920368,-1.46918830920368));
#2224=CARTESIAN_POINT('Origin',(11.,-1.90918830920368,-1.90918830920368));
#2225=CARTESIAN_POINT('Origin',(10.1,-1.90918830920368,1.90918830920368));
#2226=CARTESIAN_POINT('',(10.2,-1.90918830920368,2.34918830920368));
#2227=CARTESIAN_POINT('Origin',(10.2,-1.90918830920368,1.90918830920368));
#2228=CARTESIAN_POINT('',(11.,-1.90918830920368,2.34918830920368));
#2229=CARTESIAN_POINT('',(10.1,-1.90918830920368,2.34918830920368));
#2230=CARTESIAN_POINT('Origin',(11.,-1.90918830920368,1.90918830920368));
#2231=CARTESIAN_POINT('Origin',(10.1,1.90918830920368,1.90918830920368));
#2232=CARTESIAN_POINT('',(10.2,1.90918830920368,2.34918830920368));
#2233=CARTESIAN_POINT('Origin',(10.2,1.90918830920368,1.90918830920368));
#2234=CARTESIAN_POINT('',(11.,1.90918830920368,2.34918830920368));
#2235=CARTESIAN_POINT('',(10.1,1.90918830920368,2.34918830920368));
#2236=CARTESIAN_POINT('Origin',(11.,1.90918830920368,1.90918830920368));
#2237=CARTESIAN_POINT('Origin',(10.1,1.90918830920368,-1.90918830920368));
#2238=CARTESIAN_POINT('',(10.2,1.90918830920368,-1.46918830920368));
#2239=CARTESIAN_POINT('Origin',(10.2,1.90918830920368,-1.90918830920368));
#2240=CARTESIAN_POINT('',(11.,1.90918830920368,-1.46918830920368));
#2241=CARTESIAN_POINT('',(10.1,1.90918830920368,-1.46918830920368));
#2242=CARTESIAN_POINT('Origin',(11.,1.90918830920368,-1.90918830920368));
#2243=CARTESIAN_POINT('Origin',(10.2,0.,0.));
#2244=CARTESIAN_POINT('',(11.,-1.30424884109193E-16,1.065));
#2245=CARTESIAN_POINT('Origin',(11.,0.,0.));
#2246=CARTESIAN_POINT('',(10.2,-1.30424884109193E-16,1.065));
#2247=CARTESIAN_POINT('',(10.2,-1.30424884109193E-16,1.065));
#2248=CARTESIAN_POINT('Origin',(10.2,0.,0.));
#2249=CARTESIAN_POINT('Origin',(10.2,0.,0.));
#2250=CARTESIAN_POINT('',(11.,-4.28626379701574E-16,3.5));
#2251=CARTESIAN_POINT('Origin',(11.,0.,0.));
#2252=CARTESIAN_POINT('',(10.2,-4.28626379701574E-16,3.5));
#2253=CARTESIAN_POINT('',(10.2,-4.28626379701574E-16,3.5));
#2254=CARTESIAN_POINT('Origin',(10.2,0.,0.));
#2255=CARTESIAN_POINT('Origin',(11.,0.,0.));
#2256=CARTESIAN_POINT('Origin',(10.2,0.,0.));
#2257=CARTESIAN_POINT('',(0.,0.,0.));
#2258=CARTESIAN_POINT('Origin',(-10.2,0.,0.));
#2259=CARTESIAN_POINT('',(-10.,-1.30424884109193E-16,1.065));
#2260=CARTESIAN_POINT('Origin',(-10.,0.,0.));
#2261=CARTESIAN_POINT('',(-10.2,-1.30424884109193E-16,1.065));
#2262=CARTESIAN_POINT('',(-10.2,-1.30424884109193E-16,1.065));
#2263=CARTESIAN_POINT('Origin',(-10.2,0.,0.));
#2264=CARTESIAN_POINT('Origin',(-10.2,0.,0.));
#2265=CARTESIAN_POINT('',(-10.,-2.69422295812418E-16,2.2));
#2266=CARTESIAN_POINT('Origin',(-10.,0.,0.));
#2267=CARTESIAN_POINT('',(-10.2,-2.69422295812418E-16,2.2));
#2268=CARTESIAN_POINT('',(-10.2,-2.69422295812418E-16,2.2));
#2269=CARTESIAN_POINT('Origin',(-10.2,0.,0.));
#2270=CARTESIAN_POINT('Origin',(-10.,0.,0.));
#2271=CARTESIAN_POINT('Origin',(-10.2,0.,0.));
#2272=CARTESIAN_POINT('',(0.,0.,0.));
#2273=CARTESIAN_POINT('Origin',(10.,0.,0.));
#2274=CARTESIAN_POINT('',(10.2,-1.30424884109193E-16,1.065));
#2275=CARTESIAN_POINT('Origin',(10.2,0.,0.));
#2276=CARTESIAN_POINT('',(10.,-1.30424884109193E-16,1.065));
#2277=CARTESIAN_POINT('',(10.,-1.30424884109193E-16,1.065));
#2278=CARTESIAN_POINT('Origin',(10.,0.,0.));
#2279=CARTESIAN_POINT('Origin',(10.,0.,0.));
#2280=CARTESIAN_POINT('',(10.2,-2.69422295812418E-16,2.2));
#2281=CARTESIAN_POINT('Origin',(10.2,0.,0.));
#2282=CARTESIAN_POINT('',(10.,-2.69422295812418E-16,2.2));
#2283=CARTESIAN_POINT('',(10.,-2.69422295812418E-16,2.2));
#2284=CARTESIAN_POINT('Origin',(10.,0.,0.));
#2285=CARTESIAN_POINT('Origin',(10.2,0.,0.));
#2286=CARTESIAN_POINT('Origin',(10.,0.,0.));
#2287=CARTESIAN_POINT('',(0.,0.,0.));
#2288=CARTESIAN_POINT('Origin',(0.,-1.935,0.));
#2289=CARTESIAN_POINT('',(-0.3933,-3.9267,4.81653586104654E-17));
#2290=CARTESIAN_POINT('Origin',(0.,-3.9267,0.));
#2291=CARTESIAN_POINT('',(-0.3933,0.,-4.81653586104654E-17));
#2292=CARTESIAN_POINT('',(-0.3933,-1.935,-4.81653586104654E-17));
#2293=CARTESIAN_POINT('Origin',(0.,0.,0.));
#2294=CARTESIAN_POINT('Origin',(0.,-3.96,0.));
#2295=CARTESIAN_POINT('',(-0.32,-4.,-3.91886975727153E-17));
#2296=CARTESIAN_POINT('Origin',(0.,-4.,0.));
#2297=CARTESIAN_POINT('',(-0.36,-3.96,-4.40872847693047E-17));
#2298=CARTESIAN_POINT('Origin',(0.,-4.,0.));
#2299=CARTESIAN_POINT('Origin',(0.,0.462722715486149,0.));
#2300=CARTESIAN_POINT('',(-0.6175,0.53,-7.5621939847349E-17));
#2301=CARTESIAN_POINT('Origin',(0.,0.53,0.));
#2302=CARTESIAN_POINT('',(-0.750555349946514,0.453180457891261,-9.19165206894919E-17));
#2303=CARTESIAN_POINT('',(-0.734027674973257,0.462722715486149,-8.98924642641573E-17));
#2304=CARTESIAN_POINT('',(-0.375277674973257,0.453180457891261,0.65));
#2305=CARTESIAN_POINT('Ctrl Pts',(-0.375277674973257,0.45318045789126,0.65));
#2306=CARTESIAN_POINT('Ctrl Pts',(-0.562916512459968,0.561513791224244,
0.324999999999856));
#2307=CARTESIAN_POINT('Ctrl Pts',(-0.750555349946514,0.45318045789126,-9.19165206894919E-17));
#2308=CARTESIAN_POINT('',(0.375277674973257,0.453180457891261,0.65));
#2309=CARTESIAN_POINT('Ctrl Pts',(0.375277674973257,0.453180457891261,0.65));
#2310=CARTESIAN_POINT('Ctrl Pts',(-1.66922031752392E-13,0.561513791224244,
0.65));
#2311=CARTESIAN_POINT('Ctrl Pts',(-0.375277674973257,0.45318045789126,0.65));
#2312=CARTESIAN_POINT('',(0.750555349946514,0.453180457891261,0.));
#2313=CARTESIAN_POINT('Ctrl Pts',(0.750555349946514,0.453180457891261,0.));
#2314=CARTESIAN_POINT('Ctrl Pts',(0.562916512459802,0.561513791224244,0.325000000000144));
#2315=CARTESIAN_POINT('Ctrl Pts',(0.375277674973257,0.45318045789126,0.65));
#2316=CARTESIAN_POINT('',(0.375277674973257,0.453180457891261,-0.65));
#2317=CARTESIAN_POINT('Ctrl Pts',(0.375277674973257,0.45318045789126,-0.65));
#2318=CARTESIAN_POINT('Ctrl Pts',(0.562916512459968,0.561513791224244,-0.324999999999855));
#2319=CARTESIAN_POINT('Ctrl Pts',(0.750555349946514,0.453180457891261,0.));
#2320=CARTESIAN_POINT('',(-0.375277674973257,0.45318045789126,-0.65));
#2321=CARTESIAN_POINT('Ctrl Pts',(-0.375277674973257,0.453180457891261,
-0.65));
#2322=CARTESIAN_POINT('Ctrl Pts',(1.66866520601161E-13,0.561513791224244,
-0.65));
#2323=CARTESIAN_POINT('Ctrl Pts',(0.375277674973257,0.45318045789126,-0.65));
#2324=CARTESIAN_POINT('Ctrl Pts',(-0.750555349946514,0.453180457891261,
-9.19165206894919E-17));
#2325=CARTESIAN_POINT('Ctrl Pts',(-0.562916512459802,0.561513791224244,
-0.325000000000144));
#2326=CARTESIAN_POINT('Ctrl Pts',(-0.375277674973257,0.45318045789126,-0.65));
#2327=CARTESIAN_POINT('Origin',(0.375277674973257,0.,-0.65));
#2328=CARTESIAN_POINT('',(0.375277674973257,0.,-0.65));
#2329=CARTESIAN_POINT('',(0.375277674973257,0.,-0.65));
#2330=CARTESIAN_POINT('',(-0.375277674973257,0.,-0.65));
#2331=CARTESIAN_POINT('',(0.375277674973257,0.,-0.65));
#2332=CARTESIAN_POINT('',(-0.375277674973257,0.,-0.65));
#2333=CARTESIAN_POINT('Origin',(0.750555349946514,0.,0.));
#2334=CARTESIAN_POINT('',(0.750555349946514,0.,0.));
#2335=CARTESIAN_POINT('',(0.750555349946514,0.,0.));
#2336=CARTESIAN_POINT('',(0.750555349946514,0.,0.));
#2337=CARTESIAN_POINT('Origin',(0.375277674973257,0.,0.65));
#2338=CARTESIAN_POINT('',(0.375277674973257,0.,0.65));
#2339=CARTESIAN_POINT('',(0.375277674973257,0.,0.65));
#2340=CARTESIAN_POINT('',(0.375277674973257,0.,0.65));
#2341=CARTESIAN_POINT('Origin',(-0.375277674973257,0.,0.65));
#2342=CARTESIAN_POINT('',(-0.375277674973257,0.,0.65));
#2343=CARTESIAN_POINT('',(-0.375277674973257,0.,0.65));
#2344=CARTESIAN_POINT('',(-0.375277674973257,0.,0.65));
#2345=CARTESIAN_POINT('Origin',(-0.750555349946514,0.,-9.19165206894919E-17));
#2346=CARTESIAN_POINT('',(-0.750555349946514,0.,-9.19165206894919E-17));
#2347=CARTESIAN_POINT('',(-0.750555349946514,0.,-9.19165206894919E-17));
#2348=CARTESIAN_POINT('',(-0.750555349946514,0.,-9.19165206894919E-17));
#2349=CARTESIAN_POINT('Origin',(-0.375277674973257,0.,-0.65));
#2350=CARTESIAN_POINT('',(-0.375277674973257,0.,-0.65));
#2351=CARTESIAN_POINT('Origin',(0.,0.53,-1.11022302462516E-16));
#2352=CARTESIAN_POINT('Origin',(0.,0.,-1.11022302462516E-16));
#2353=CARTESIAN_POINT('',(0.,0.,0.));
#2354=CARTESIAN_POINT('Origin',(0.,0.,0.));
#2355=CARTESIAN_POINT('',(-0.42,0.16,5.14351655641888E-17));
#2356=CARTESIAN_POINT('Origin',(0.,0.16,0.));
#2357=CARTESIAN_POINT('',(-0.42,0.,5.14351655641888E-17));
#2358=CARTESIAN_POINT('',(-0.42,0.,5.14351655641888E-17));
#2359=CARTESIAN_POINT('Origin',(0.,0.,0.));
#2360=CARTESIAN_POINT('Origin',(0.,0.,0.));
#2361=CARTESIAN_POINT('',(-0.8,0.16,9.79717439317883E-17));
#2362=CARTESIAN_POINT('Origin',(0.,0.16,0.));
#2363=CARTESIAN_POINT('',(-0.8,0.,9.79717439317883E-17));
#2364=CARTESIAN_POINT('',(-0.8,0.,9.79717439317883E-17));
#2365=CARTESIAN_POINT('Origin',(0.,0.,0.));
#2366=CARTESIAN_POINT('Origin',(0.,0.16,0.));
#2367=CARTESIAN_POINT('Origin',(0.,0.,0.));
#2368=CARTESIAN_POINT('',(0.,0.,0.));
#2369=CARTESIAN_POINT('Origin',(0.,0.067277284513851,0.));
#2370=CARTESIAN_POINT('',(-0.375277674973257,0.0768195421087395,0.65));
#2371=CARTESIAN_POINT('',(0.375277674973257,0.0768195421087395,0.65));
#2372=CARTESIAN_POINT('Ctrl Pts',(-0.375277674973257,0.0768195421087395,
0.65));
#2373=CARTESIAN_POINT('Ctrl Pts',(1.66533453693773E-13,-0.0315137912242439,
0.65));
#2374=CARTESIAN_POINT('Ctrl Pts',(0.375277674973257,0.0768195421087394,
0.65));
#2375=CARTESIAN_POINT('',(-0.750555349946514,0.0768195421087394,-9.19165206894919E-17));
#2376=CARTESIAN_POINT('Ctrl Pts',(-0.750555349946514,0.0768195421087394,
-9.19165206894919E-17));
#2377=CARTESIAN_POINT('Ctrl Pts',(-0.562916512459802,-0.0315137912242434,
0.325000000000144));
#2378=CARTESIAN_POINT('Ctrl Pts',(-0.375277674973257,0.0768195421087395,
0.65));
#2379=CARTESIAN_POINT('',(-0.6175,-2.77555756156289E-17,-7.5621939847349E-17));
#2380=CARTESIAN_POINT('',(-0.734027674973257,0.067277284513851,-8.98924642641573E-17));
#2381=CARTESIAN_POINT('Origin',(0.,0.,0.));
#2382=CARTESIAN_POINT('',(-0.375277674973257,0.0768195421087395,-0.65));
#2383=CARTESIAN_POINT('Ctrl Pts',(-0.375277674973257,0.0768195421087395,
-0.65));
#2384=CARTESIAN_POINT('Ctrl Pts',(-0.562916512459968,-0.0315137912242437,
-0.324999999999856));
#2385=CARTESIAN_POINT('Ctrl Pts',(-0.750555349946514,0.0768195421087395,
-9.19165206894919E-17));
#2386=CARTESIAN_POINT('',(0.375277674973257,0.0768195421087395,-0.65));
#2387=CARTESIAN_POINT('Ctrl Pts',(0.375277674973257,0.0768195421087395,
-0.65));
#2388=CARTESIAN_POINT('Ctrl Pts',(-1.66144875635155E-13,-0.0315137912242437,
-0.65));
#2389=CARTESIAN_POINT('Ctrl Pts',(-0.375277674973257,0.0768195421087395,
-0.65));
#2390=CARTESIAN_POINT('',(0.750555349946514,0.0768195421087394,0.));
#2391=CARTESIAN_POINT('Ctrl Pts',(0.750555349946514,0.0768195421087394,
0.));
#2392=CARTESIAN_POINT('Ctrl Pts',(0.562916512459802,-0.0315137912242436,
-0.325000000000144));
#2393=CARTESIAN_POINT('Ctrl Pts',(0.375277674973257,0.0768195421087395,
-0.65));
#2394=CARTESIAN_POINT('Ctrl Pts',(0.375277674973257,0.0768195421087394,
0.65));
#2395=CARTESIAN_POINT('Ctrl Pts',(0.562916512459968,-0.0315137912242439,
0.324999999999856));
#2396=CARTESIAN_POINT('Ctrl Pts',(0.750555349946514,0.0768195421087394,
0.));
#2397=CARTESIAN_POINT('Origin',(0.,0.612722715486149,0.));
#2398=CARTESIAN_POINT('',(-0.6175,0.68,-7.5621939847349E-17));
#2399=CARTESIAN_POINT('Origin',(0.,0.68,0.));
#2400=CARTESIAN_POINT('',(-0.750555349946514,0.603180457891261,-9.19165206894919E-17));
#2401=CARTESIAN_POINT('',(-0.734027674973257,0.612722715486149,-8.98924642641573E-17));
#2402=CARTESIAN_POINT('',(-0.375277674973257,0.603180457891261,0.65));
#2403=CARTESIAN_POINT('Ctrl Pts',(-0.375277674973257,0.603180457891261,
0.65));
#2404=CARTESIAN_POINT('Ctrl Pts',(-0.562916512459968,0.711513791224243,
0.324999999999856));
#2405=CARTESIAN_POINT('Ctrl Pts',(-0.750555349946514,0.603180457891261,
-9.19165206894919E-17));
#2406=CARTESIAN_POINT('',(0.375277674973257,0.603180457891261,0.65));
#2407=CARTESIAN_POINT('Ctrl Pts',(0.375277674973257,0.603180457891261,0.65));
#2408=CARTESIAN_POINT('Ctrl Pts',(-1.66755498298699E-13,0.711513791224244,
0.65));
#2409=CARTESIAN_POINT('Ctrl Pts',(-0.375277674973257,0.603180457891261,
0.65));
#2410=CARTESIAN_POINT('',(0.750555349946514,0.603180457891261,0.));
#2411=CARTESIAN_POINT('Ctrl Pts',(0.750555349946514,0.603180457891261,0.));
#2412=CARTESIAN_POINT('Ctrl Pts',(0.562916512459802,0.711513791224244,0.325000000000144));
#2413=CARTESIAN_POINT('Ctrl Pts',(0.375277674973257,0.603180457891261,0.65));
#2414=CARTESIAN_POINT('',(0.375277674973257,0.603180457891261,-0.65));
#2415=CARTESIAN_POINT('Ctrl Pts',(0.375277674973257,0.603180457891261,-0.65));
#2416=CARTESIAN_POINT('Ctrl Pts',(0.562916512459969,0.711513791224244,-0.324999999999856));
#2417=CARTESIAN_POINT('Ctrl Pts',(0.750555349946514,0.603180457891261,0.));
#2418=CARTESIAN_POINT('',(-0.375277674973257,0.603180457891261,-0.65));
#2419=CARTESIAN_POINT('Ctrl Pts',(-0.375277674973257,0.603180457891261,
-0.65));
#2420=CARTESIAN_POINT('Ctrl Pts',(1.66422431391311E-13,0.711513791224244,
-0.65));
#2421=CARTESIAN_POINT('Ctrl Pts',(0.375277674973257,0.603180457891261,-0.65));
#2422=CARTESIAN_POINT('Ctrl Pts',(-0.750555349946514,0.603180457891261,
-9.19165206894919E-17));
#2423=CARTESIAN_POINT('Ctrl Pts',(-0.562916512459802,0.711513791224244,
-0.325000000000144));
#2424=CARTESIAN_POINT('Ctrl Pts',(-0.375277674973257,0.603180457891261,
-0.65));
#2425=CARTESIAN_POINT('Origin',(0.375277674973257,0.,-0.65));
#2426=CARTESIAN_POINT('',(-0.375277674973257,0.,-0.65));
#2427=CARTESIAN_POINT('',(0.375277674973257,0.,-0.65));
#2428=CARTESIAN_POINT('Origin',(-0.375277674973257,0.,-0.65));
#2429=CARTESIAN_POINT('',(-0.750555349946514,0.,-9.19165206894919E-17));
#2430=CARTESIAN_POINT('Origin',(-0.750555349946514,0.,-9.19165206894919E-17));
#2431=CARTESIAN_POINT('',(-0.375277674973257,0.,0.65));
#2432=CARTESIAN_POINT('Origin',(0.,0.,0.));
#2433=CARTESIAN_POINT('',(-0.338975,0.68,4.15124648740974E-17));
#2434=CARTESIAN_POINT('Origin',(0.,0.68,0.));
#2435=CARTESIAN_POINT('',(-0.338975,0.,4.15124648740974E-17));
#2436=CARTESIAN_POINT('',(-0.338975,0.,4.15124648740974E-17));
#2437=CARTESIAN_POINT('Origin',(0.,0.,0.));
#2438=CARTESIAN_POINT('Origin',(-0.375277674973257,0.,0.65));
#2439=CARTESIAN_POINT('',(0.375277674973257,0.,0.65));
#2440=CARTESIAN_POINT('Origin',(0.750555349946514,0.,0.));
#2441=CARTESIAN_POINT('',(0.750555349946514,0.,0.));
#2442=CARTESIAN_POINT('Origin',(0.375277674973257,0.,0.65));
#2443=CARTESIAN_POINT('Origin',(0.,0.68,-1.11022302462516E-16));
#2444=CARTESIAN_POINT('Origin',(0.,0.,-1.11022302462516E-16));
#2445=CARTESIAN_POINT('',(0.,0.,0.));
#2446=CARTESIAN_POINT('',(0.,0.,0.));
#2447=CARTESIAN_POINT('',(0.,0.,0.));
#2448=CARTESIAN_POINT('',(0.,0.,0.));
#2449=CARTESIAN_POINT('',(0.,0.,0.));
#2450=CARTESIAN_POINT('',(0.,0.,0.));
#2451=CARTESIAN_POINT('',(0.,0.,0.));
#2452=CARTESIAN_POINT('',(-11.16,1.90918830920368,1.90918830920368));
#2453=CARTESIAN_POINT('',(-11.16,1.90918830920368,1.90918830920368));
#2454=CARTESIAN_POINT('',(-9.2,1.90918830920368,1.90918830920368));
#2455=CARTESIAN_POINT('',(-9.04,1.90918830920368,1.90918830920368));
#2456=CARTESIAN_POINT('',(-11.16,-1.90918830920368,1.90918830920368));
#2457=CARTESIAN_POINT('',(-11.16,-1.90918830920368,1.90918830920368));
#2458=CARTESIAN_POINT('',(-9.2,-1.90918830920368,1.90918830920368));
#2459=CARTESIAN_POINT('',(-9.04,-1.90918830920368,1.90918830920368));
#2460=CARTESIAN_POINT('',(-11.16,-1.90918830920368,-1.90918830920368));
#2461=CARTESIAN_POINT('',(-11.16,-1.90918830920368,-1.90918830920368));
#2462=CARTESIAN_POINT('',(-9.2,-1.90918830920368,-1.90918830920368));
#2463=CARTESIAN_POINT('',(-9.04,-1.90918830920368,-1.90918830920368));
#2464=CARTESIAN_POINT('',(-11.16,1.90918830920368,-1.90918830920368));
#2465=CARTESIAN_POINT('',(-11.16,1.90918830920368,-1.90918830920368));
#2466=CARTESIAN_POINT('',(-9.2,1.90918830920368,-1.90918830920368));
#2467=CARTESIAN_POINT('',(-9.04,1.90918830920368,-1.90918830920368));
#2468=CARTESIAN_POINT('',(9.04,1.90918830920368,1.90918830920368));
#2469=CARTESIAN_POINT('',(9.04,1.90918830920368,1.90918830920368));
#2470=CARTESIAN_POINT('',(11.,1.90918830920368,1.90918830920368));
#2471=CARTESIAN_POINT('',(11.16,1.90918830920368,1.90918830920368));
#2472=CARTESIAN_POINT('',(9.04,-1.90918830920368,1.90918830920368));
#2473=CARTESIAN_POINT('',(9.04,-1.90918830920368,1.90918830920368));
#2474=CARTESIAN_POINT('',(11.,-1.90918830920368,1.90918830920368));
#2475=CARTESIAN_POINT('',(11.16,-1.90918830920368,1.90918830920368));
#2476=CARTESIAN_POINT('',(9.04,-1.90918830920368,-1.90918830920368));
#2477=CARTESIAN_POINT('',(9.04,-1.90918830920368,-1.90918830920368));
#2478=CARTESIAN_POINT('',(11.,-1.90918830920368,-1.90918830920368));
#2479=CARTESIAN_POINT('',(11.16,-1.90918830920368,-1.90918830920368));
#2480=CARTESIAN_POINT('',(9.04,1.90918830920368,-1.90918830920368));
#2481=CARTESIAN_POINT('',(9.04,1.90918830920368,-1.90918830920368));
#2482=CARTESIAN_POINT('',(11.,1.90918830920368,-1.90918830920368));
#2483=CARTESIAN_POINT('',(11.16,1.90918830920368,-1.90918830920368));
#2484=UNCERTAINTY_MEASURE_WITH_UNIT(LENGTH_MEASURE(0.001),#2508,
'DISTANCE_ACCURACY_VALUE',
'Maximum model space distance between geometric entities at asserted c
onnectivities');
#2485=UNCERTAINTY_MEASURE_WITH_UNIT(LENGTH_MEASURE(0.001),#2508,
'DISTANCE_ACCURACY_VALUE',
'Maximum model space distance between geometric entities at asserted c
onnectivities');
#2486=UNCERTAINTY_MEASURE_WITH_UNIT(LENGTH_MEASURE(0.001),#2508,
'DISTANCE_ACCURACY_VALUE',
'Maximum model space distance between geometric entities at asserted c
onnectivities');
#2487=UNCERTAINTY_MEASURE_WITH_UNIT(LENGTH_MEASURE(0.001),#2508,
'DISTANCE_ACCURACY_VALUE',
'Maximum model space distance between geometric entities at asserted c
onnectivities');
#2488=UNCERTAINTY_MEASURE_WITH_UNIT(LENGTH_MEASURE(0.001),#2508,
'DISTANCE_ACCURACY_VALUE',
'Maximum model space distance between geometric entities at asserted c
onnectivities');
#2489=UNCERTAINTY_MEASURE_WITH_UNIT(LENGTH_MEASURE(0.001),#2508,
'DISTANCE_ACCURACY_VALUE',
'Maximum model space distance between geometric entities at asserted c
onnectivities');
#2490=UNCERTAINTY_MEASURE_WITH_UNIT(LENGTH_MEASURE(0.001),#2508,
'DISTANCE_ACCURACY_VALUE',
'Maximum model space distance between geometric entities at asserted c
onnectivities');
#2491=UNCERTAINTY_MEASURE_WITH_UNIT(LENGTH_MEASURE(0.001),#2508,
'DISTANCE_ACCURACY_VALUE',
'Maximum model space distance between geometric entities at asserted c
onnectivities');
#2492=UNCERTAINTY_MEASURE_WITH_UNIT(LENGTH_MEASURE(0.001),#2508,
'DISTANCE_ACCURACY_VALUE',
'Maximum model space distance between geometric entities at asserted c
onnectivities');
#2493=UNCERTAINTY_MEASURE_WITH_UNIT(LENGTH_MEASURE(0.001),#2508,
'DISTANCE_ACCURACY_VALUE',
'Maximum model space distance between geometric entities at asserted c
onnectivities');
#2494=UNCERTAINTY_MEASURE_WITH_UNIT(LENGTH_MEASURE(0.001),#2508,
'DISTANCE_ACCURACY_VALUE',
'Maximum model space distance between geometric entities at asserted c
onnectivities');
#2495=UNCERTAINTY_MEASURE_WITH_UNIT(LENGTH_MEASURE(0.001),#2508,
'DISTANCE_ACCURACY_VALUE',
'Maximum model space distance between geometric entities at asserted c
onnectivities');
#2496=(
GEOMETRIC_REPRESENTATION_CONTEXT(3)
GLOBAL_UNCERTAINTY_ASSIGNED_CONTEXT((#2484))
GLOBAL_UNIT_ASSIGNED_CONTEXT((#2508,#2510,#2511))
REPRESENTATION_CONTEXT('','3D')
);
#2497=(
GEOMETRIC_REPRESENTATION_CONTEXT(3)
GLOBAL_UNCERTAINTY_ASSIGNED_CONTEXT((#2485))
GLOBAL_UNIT_ASSIGNED_CONTEXT((#2508,#2510,#2511))
REPRESENTATION_CONTEXT('','3D')
);
#2498=(
GEOMETRIC_REPRESENTATION_CONTEXT(3)
GLOBAL_UNCERTAINTY_ASSIGNED_CONTEXT((#2486))
GLOBAL_UNIT_ASSIGNED_CONTEXT((#2508,#2510,#2511))
REPRESENTATION_CONTEXT('','3D')
);
#2499=(
GEOMETRIC_REPRESENTATION_CONTEXT(3)
GLOBAL_UNCERTAINTY_ASSIGNED_CONTEXT((#2487))
GLOBAL_UNIT_ASSIGNED_CONTEXT((#2508,#2510,#2511))
REPRESENTATION_CONTEXT('','3D')
);
#2500=(
GEOMETRIC_REPRESENTATION_CONTEXT(3)
GLOBAL_UNCERTAINTY_ASSIGNED_CONTEXT((#2488))
GLOBAL_UNIT_ASSIGNED_CONTEXT((#2508,#2510,#2511))
REPRESENTATION_CONTEXT('','3D')
);
#2501=(
GEOMETRIC_REPRESENTATION_CONTEXT(3)
GLOBAL_UNCERTAINTY_ASSIGNED_CONTEXT((#2489))
GLOBAL_UNIT_ASSIGNED_CONTEXT((#2508,#2510,#2511))
REPRESENTATION_CONTEXT('','3D')
);
#2502=(
GEOMETRIC_REPRESENTATION_CONTEXT(3)
GLOBAL_UNCERTAINTY_ASSIGNED_CONTEXT((#2490))
GLOBAL_UNIT_ASSIGNED_CONTEXT((#2508,#2510,#2511))
REPRESENTATION_CONTEXT('','3D')
);
#2503=(
GEOMETRIC_REPRESENTATION_CONTEXT(3)
GLOBAL_UNCERTAINTY_ASSIGNED_CONTEXT((#2491))
GLOBAL_UNIT_ASSIGNED_CONTEXT((#2508,#2510,#2511))
REPRESENTATION_CONTEXT('','3D')
);
#2504=(
GEOMETRIC_REPRESENTATION_CONTEXT(3)
GLOBAL_UNCERTAINTY_ASSIGNED_CONTEXT((#2492))
GLOBAL_UNIT_ASSIGNED_CONTEXT((#2508,#2510,#2511))
REPRESENTATION_CONTEXT('','3D')
);
#2505=(
GEOMETRIC_REPRESENTATION_CONTEXT(3)
GLOBAL_UNCERTAINTY_ASSIGNED_CONTEXT((#2493))
GLOBAL_UNIT_ASSIGNED_CONTEXT((#2508,#2510,#2511))
REPRESENTATION_CONTEXT('','3D')
);
#2506=(
GEOMETRIC_REPRESENTATION_CONTEXT(3)
GLOBAL_UNCERTAINTY_ASSIGNED_CONTEXT((#2494))
GLOBAL_UNIT_ASSIGNED_CONTEXT((#2508,#2510,#2511))
REPRESENTATION_CONTEXT('','3D')
);
#2507=(
GEOMETRIC_REPRESENTATION_CONTEXT(3)
GLOBAL_UNCERTAINTY_ASSIGNED_CONTEXT((#2495))
GLOBAL_UNIT_ASSIGNED_CONTEXT((#2508,#2510,#2511))
REPRESENTATION_CONTEXT('','3D')
);
#2508=(
LENGTH_UNIT()
NAMED_UNIT(*)
SI_UNIT(.CENTI.,.METRE.)
);
#2509=(
LENGTH_UNIT()
NAMED_UNIT(*)
SI_UNIT($,.METRE.)
);
#2510=(
NAMED_UNIT(*)
PLANE_ANGLE_UNIT()
SI_UNIT($,.RADIAN.)
);
#2511=(
NAMED_UNIT(*)
SI_UNIT($,.STERADIAN.)
SOLID_ANGLE_UNIT()
);
#2512=SHAPE_DEFINITION_REPRESENTATION(#2523,#2573);
#2513=SHAPE_DEFINITION_REPRESENTATION(#2524,#2574);
#2514=SHAPE_DEFINITION_REPRESENTATION(#2525,#2575);
#2515=SHAPE_DEFINITION_REPRESENTATION(#2526,#2576);
#2516=SHAPE_DEFINITION_REPRESENTATION(#2527,#2577);
#2517=SHAPE_DEFINITION_REPRESENTATION(#2528,#2578);
#2518=SHAPE_DEFINITION_REPRESENTATION(#2529,#2579);
#2519=SHAPE_DEFINITION_REPRESENTATION(#2530,#2580);
#2520=SHAPE_DEFINITION_REPRESENTATION(#2531,#2581);
#2521=SHAPE_DEFINITION_REPRESENTATION(#2532,#2582);
#2522=SHAPE_DEFINITION_REPRESENTATION(#2533,#2583);
#2523=PRODUCT_DEFINITION_SHAPE('',$,#2585);
#2524=PRODUCT_DEFINITION_SHAPE('',$,#2586);
#2525=PRODUCT_DEFINITION_SHAPE('',$,#2587);
#2526=PRODUCT_DEFINITION_SHAPE('',$,#2588);
#2527=PRODUCT_DEFINITION_SHAPE('',$,#2589);
#2528=PRODUCT_DEFINITION_SHAPE('',$,#2590);
#2529=PRODUCT_DEFINITION_SHAPE('',$,#2591);
#2530=PRODUCT_DEFINITION_SHAPE('',$,#2592);
#2531=PRODUCT_DEFINITION_SHAPE('',$,#2593);
#2532=PRODUCT_DEFINITION_SHAPE('',$,#2594);
#2533=PRODUCT_DEFINITION_SHAPE('',$,#2595);
#2534=PRODUCT_DEFINITION_SHAPE($,$,#128);
#2535=PRODUCT_DEFINITION_SHAPE($,$,#129);
#2536=PRODUCT_DEFINITION_SHAPE($,$,#130);
#2537=PRODUCT_DEFINITION_SHAPE($,$,#131);
#2538=PRODUCT_DEFINITION_SHAPE($,$,#132);
#2539=PRODUCT_DEFINITION_SHAPE($,$,#133);
#2540=PRODUCT_DEFINITION_SHAPE($,$,#134);
#2541=PRODUCT_DEFINITION_SHAPE($,$,#135);
#2542=PRODUCT_DEFINITION_SHAPE($,$,#136);
#2543=PRODUCT_DEFINITION_SHAPE($,$,#137);
#2544=PRODUCT_DEFINITION_SHAPE($,$,#138);
#2545=PRODUCT_DEFINITION_SHAPE($,$,#139);
#2546=PRODUCT_DEFINITION_SHAPE($,$,#140);
#2547=PRODUCT_DEFINITION_SHAPE($,$,#141);
#2548=PRODUCT_DEFINITION_SHAPE($,$,#142);
#2549=PRODUCT_DEFINITION_SHAPE($,$,#143);
#2550=PRODUCT_DEFINITION_SHAPE($,$,#144);
#2551=PRODUCT_DEFINITION_SHAPE($,$,#145);
#2552=PRODUCT_DEFINITION_SHAPE($,$,#146);
#2553=PRODUCT_DEFINITION_SHAPE($,$,#147);
#2554=PRODUCT_DEFINITION_SHAPE($,$,#148);
#2555=PRODUCT_DEFINITION_SHAPE($,$,#149);
#2556=PRODUCT_DEFINITION_SHAPE($,$,#150);
#2557=PRODUCT_DEFINITION_SHAPE($,$,#151);
#2558=PRODUCT_DEFINITION_SHAPE($,$,#152);
#2559=PRODUCT_DEFINITION_SHAPE($,$,#153);
#2560=PRODUCT_DEFINITION_SHAPE($,$,#154);
#2561=PRODUCT_DEFINITION_SHAPE($,$,#155);
#2562=PRODUCT_DEFINITION_SHAPE($,$,#156);
#2563=PRODUCT_DEFINITION_SHAPE($,$,#157);
#2564=PRODUCT_DEFINITION_SHAPE($,$,#158);
#2565=PRODUCT_DEFINITION_SHAPE($,$,#159);
#2566=PRODUCT_DEFINITION_SHAPE($,$,#160);
#2567=PRODUCT_DEFINITION_SHAPE($,$,#161);
#2568=PRODUCT_DEFINITION_SHAPE($,$,#162);
#2569=PRODUCT_DEFINITION_SHAPE($,$,#163);
#2570=PRODUCT_DEFINITION_SHAPE($,$,#164);
#2571=PRODUCT_DEFINITION_SHAPE($,$,#165);
#2572=PRODUCT_DEFINITION_SHAPE($,$,#166);
#2573=SHAPE_REPRESENTATION('',(#1450,#1604,#1605,#1606,#1607,#1608,#1609,
#1610,#1611,#1612,#1613,#1614,#1615,#1616,#1617,#1618,#1619,#1620,#1621,
#1622,#1623,#1624,#1625,#1626,#1627,#1628,#1629,#1630,#1631,#1632,#1633,
#1634,#1635,#1636,#1637,#1638,#1639,#1640,#1641,#1642),#2496);
#2574=SHAPE_REPRESENTATION('',(#1451),#2497);
#2575=SHAPE_REPRESENTATION('',(#1460),#2498);
#2576=SHAPE_REPRESENTATION('',(#1481),#2499);
#2577=SHAPE_REPRESENTATION('',(#1502),#2500);
#2578=SHAPE_REPRESENTATION('',(#1523),#2501);
#2579=SHAPE_REPRESENTATION('',(#1544),#2502);
#2580=SHAPE_REPRESENTATION('',(#1553),#2503);
#2581=SHAPE_REPRESENTATION('',(#1562),#2504);
#2582=SHAPE_REPRESENTATION('',(#1579),#2505);
#2583=SHAPE_REPRESENTATION('',(#1588),#2506);
#2584=PRODUCT_DEFINITION_CONTEXT('part definition',#2619,'design');
#2585=PRODUCT_DEFINITION('PAT-041',
'PAT-041',#2596,#2584);
#2586=PRODUCT_DEFINITION('Pipe spool','Pipe spool',#2597,#2584);
#2587=PRODUCT_DEFINITION('Weld-on flange','Weld-on flange',#2598,
#2584);
#2588=PRODUCT_DEFINITION('Weld-on flange (1)',
'Weld-on flange (1)',#2599,#2584);
#2589=PRODUCT_DEFINITION('Weld-on flange (2)','Weld-on flange (2)',
#2600,#2584);
#2590=PRODUCT_DEFINITION('Weld-on flange (3)',
'Weld-on flange (3)',#2601,#2584);
#2591=PRODUCT_DEFINITION('Flange gasket','Flange gasket',#2602,
#2584);
#2592=PRODUCT_DEFINITION('Flange gasket (1)',
'Flange gasket (1)',#2603,#2584);
#2593=PRODUCT_DEFINITION('Hex Bolt - M8x40','Hex Bolt - M8x40',
#2604,#2584);
#2594=PRODUCT_DEFINITION('Flat Washer - M8','Flat Washer - M8',
#2605,#2584);
#2595=PRODUCT_DEFINITION('Hex Nut - M8','Hex Nut - M8',#2606,
#2584);
#2596=PRODUCT_DEFINITION_FORMATION('',$,#2621);
#2597=PRODUCT_DEFINITION_FORMATION('',$,#2622);
#2598=PRODUCT_DEFINITION_FORMATION('',$,#2623);
#2599=PRODUCT_DEFINITION_FORMATION('',$,#2624);
#2600=PRODUCT_DEFINITION_FORMATION('',$,#2625);
#2601=PRODUCT_DEFINITION_FORMATION('',$,#2626);
#2602=PRODUCT_DEFINITION_FORMATION('',$,#2627);
#2603=PRODUCT_DEFINITION_FORMATION('',$,#2628);
#2604=PRODUCT_DEFINITION_FORMATION('',$,#2629);
#2605=PRODUCT_DEFINITION_FORMATION('',$,#2630);
#2606=PRODUCT_DEFINITION_FORMATION('',$,#2631);
#2607=PRODUCT_RELATED_PRODUCT_CATEGORY(
'PAT-041',
'PAT-041',(#2621));
#2608=PRODUCT_RELATED_PRODUCT_CATEGORY('Pipe spool','Pipe spool',(#2622));
#2609=PRODUCT_RELATED_PRODUCT_CATEGORY('Weld-on flange',
'Weld-on flange',(#2623));
#2610=PRODUCT_RELATED_PRODUCT_CATEGORY('Weld-on flange (1)',
'Weld-on flange (1)',(#2624));
#2611=PRODUCT_RELATED_PRODUCT_CATEGORY('Weld-on flange (2)',
'Weld-on flange (2)',(#2625));
#2612=PRODUCT_RELATED_PRODUCT_CATEGORY('Weld-on flange (3)',
'Weld-on flange (3)',(#2626));
#2613=PRODUCT_RELATED_PRODUCT_CATEGORY('Flange gasket','Flange gasket',
(#2627));
#2614=PRODUCT_RELATED_PRODUCT_CATEGORY('Flange gasket (1)',
'Flange gasket (1)',(#2628));
#2615=PRODUCT_RELATED_PRODUCT_CATEGORY('Hex Bolt - M8x40',
'Hex Bolt - M8x40',(#2629));
#2616=PRODUCT_RELATED_PRODUCT_CATEGORY('Flat Washer - M8',
'Flat Washer - M8',(#2630));
#2617=PRODUCT_RELATED_PRODUCT_CATEGORY('Hex Nut - M8','Hex Nut - M8',(#2631));
#2618=APPLICATION_PROTOCOL_DEFINITION('international standard',
'automotive_design',2009,#2619);
#2619=APPLICATION_CONTEXT(
'Core Data for Automotive Mechanical Design Process');
#2620=PRODUCT_CONTEXT('part definition',#2619,'mechanical');
#2621=PRODUCT('PAT-041',
'PAT-041',
'PAT-041',(#2620));
#2622=PRODUCT('Pipe spool','Pipe spool','Pipe spool',(#2620));
#2623=PRODUCT('Weld-on flange','Weld-on flange',
'Weld-on flange',(#2620));
#2624=PRODUCT('Weld-on flange (1)','Weld-on flange (1)',
'Weld-on flange (1)',(#2620));
#2625=PRODUCT('Weld-on flange (2)','Weld-on flange (2)',
'Weld-on flange (2)',(#2620));
#2626=PRODUCT('Weld-on flange (3)','Weld-on flange (3)',
'Weld-on flange (3)',(#2620));
#2627=PRODUCT('Flange gasket','Flange gasket',
'Flange gasket',(#2620));
#2628=PRODUCT('Flange gasket (1)','Flange gasket (1)',
'Flange gasket (1)',(#2620));
#2629=PRODUCT('Hex Bolt - M8x40','Hex Bolt - M8x40',
'Hex Bolt - M8x40',(#2620));
#2630=PRODUCT('Flat Washer - M8','Flat Washer - M8',
'Flat Washer - M8',(#2620));
#2631=PRODUCT('Hex Nut - M8','Hex Nut - M8','Hex Nut - M8',
(#2620));
#2632=PRESENTATION_STYLE_ASSIGNMENT((#2637));
#2633=PRESENTATION_STYLE_ASSIGNMENT((#2638));
#2634=PRESENTATION_STYLE_ASSIGNMENT((#2639));
#2635=PRESENTATION_STYLE_ASSIGNMENT((#2640));
#2636=PRESENTATION_STYLE_ASSIGNMENT((#2641));
#2637=SURFACE_STYLE_USAGE(.BOTH.,#2642);
#2638=SURFACE_STYLE_USAGE(.BOTH.,#2643);
#2639=SURFACE_STYLE_USAGE(.BOTH.,#2644);
#2640=SURFACE_STYLE_USAGE(.BOTH.,#2645);
#2641=SURFACE_STYLE_USAGE(.BOTH.,#2646);
#2642=SURFACE_SIDE_STYLE('',(#2647));
#2643=SURFACE_SIDE_STYLE('',(#2648));
#2644=SURFACE_SIDE_STYLE('',(#2649));
#2645=SURFACE_SIDE_STYLE('',(#2650));
#2646=SURFACE_SIDE_STYLE('',(#2651));
#2647=SURFACE_STYLE_FILL_AREA(#2652);
#2648=SURFACE_STYLE_FILL_AREA(#2653);
#2649=SURFACE_STYLE_FILL_AREA(#2654);
#2650=SURFACE_STYLE_FILL_AREA(#2655);
#2651=SURFACE_STYLE_FILL_AREA(#2656);
#2652=FILL_AREA_STYLE('Steel - Satin',(#2657));
#2653=FILL_AREA_STYLE('CAD Library Painted - Engineering blue',(#2658));
#2654=FILL_AREA_STYLE('CAD Library Painted - Off white',(#2659));
#2655=FILL_AREA_STYLE('CAD Library Painted - Graphite',(#2660));
#2656=FILL_AREA_STYLE('CAD Library Painted - Steel gray',(#2661));
#2657=FILL_AREA_STYLE_COLOUR('Steel - Satin',#2662);
#2658=FILL_AREA_STYLE_COLOUR('CAD Library Painted - Engineering blue',#2663);
#2659=FILL_AREA_STYLE_COLOUR('CAD Library Painted - Off white',#2664);
#2660=FILL_AREA_STYLE_COLOUR('CAD Library Painted - Graphite',#2665);
#2661=FILL_AREA_STYLE_COLOUR('CAD Library Painted - Steel gray',#2666);
#2662=COLOUR_RGB('Steel - Satin',0.627450980392157,0.627450980392157,0.627450980392157);
#2663=COLOUR_RGB('CAD Library Painted - Engineering blue',0.12156862745098,
0.356862745098039,0.6);
#2664=COLOUR_RGB('CAD Library Painted - Off white',0.909803921568627,0.901960784313726,
0.858823529411765);
#2665=COLOUR_RGB('CAD Library Painted - Graphite',0.0980392156862745,0.109803921568627,
0.125490196078431);
#2666=COLOUR_RGB('CAD Library Painted - Steel gray',0.592156862745098,0.631372549019608,
0.67843137254902);
#2667=COLOUR_RGB('Dark Blue',0.08,0.2,0.34);
#2668=FILL_AREA_STYLE_COLOUR('',#2667);
#2669=FILL_AREA_STYLE('',(#2668));
#2670=SURFACE_STYLE_FILL_AREA(#2669);
#2671=SURFACE_SIDE_STYLE('',(#2670));
#2672=SURFACE_STYLE_USAGE(.BOTH.,#2671);
#2673=PRESENTATION_STYLE_ASSIGNMENT((#2672));
#2674=COLOUR_RGB('Light Blue',0.38,0.62,0.78);
#2675=FILL_AREA_STYLE_COLOUR('',#2674);
#2676=FILL_AREA_STYLE('',(#2675));
#2677=SURFACE_STYLE_FILL_AREA(#2676);
#2678=SURFACE_SIDE_STYLE('',(#2677));
#2679=SURFACE_STYLE_USAGE(.BOTH.,#2678);
#2680=PRESENTATION_STYLE_ASSIGNMENT((#2679));
#2681=COLOUR_RGB('Sky Blue',0.24,0.69,0.87);
#2682=FILL_AREA_STYLE_COLOUR('',#2681);
#2683=FILL_AREA_STYLE('',(#2682));
#2684=SURFACE_STYLE_FILL_AREA(#2683);
#2685=SURFACE_SIDE_STYLE('',(#2684));
#2686=SURFACE_STYLE_USAGE(.BOTH.,#2685);
#2687=PRESENTATION_STYLE_ASSIGNMENT((#2686));
#2688=COLOUR_RGB('Grey',0.48,0.52,0.57);
#2689=FILL_AREA_STYLE_COLOUR('',#2688);
#2690=FILL_AREA_STYLE('',(#2689));
#2691=SURFACE_STYLE_FILL_AREA(#2690);
#2692=SURFACE_SIDE_STYLE('',(#2691));
#2693=SURFACE_STYLE_USAGE(.BOTH.,#2692);
#2694=PRESENTATION_STYLE_ASSIGNMENT((#2693));
#2695=COLOUR_RGB('Black',0.12,0.14,0.17);
#2696=FILL_AREA_STYLE_COLOUR('',#2695);
#2697=FILL_AREA_STYLE('',(#2696));
#2698=SURFACE_STYLE_FILL_AREA(#2697);
#2699=SURFACE_SIDE_STYLE('',(#2698));
#2700=SURFACE_STYLE_USAGE(.BOTH.,#2699);
#2701=PRESENTATION_STYLE_ASSIGNMENT((#2700));
#2702=COLOUR_RGB('Off White',0.89,0.88,0.83);
#2703=FILL_AREA_STYLE_COLOUR('',#2702);
#2704=FILL_AREA_STYLE('',(#2703));
#2705=SURFACE_STYLE_FILL_AREA(#2704);
#2706=SURFACE_SIDE_STYLE('',(#2705));
#2707=SURFACE_STYLE_USAGE(.BOTH.,#2706);
#2708=PRESENTATION_STYLE_ASSIGNMENT((#2707));
ENDSEC;
END-ISO-10303-21;
